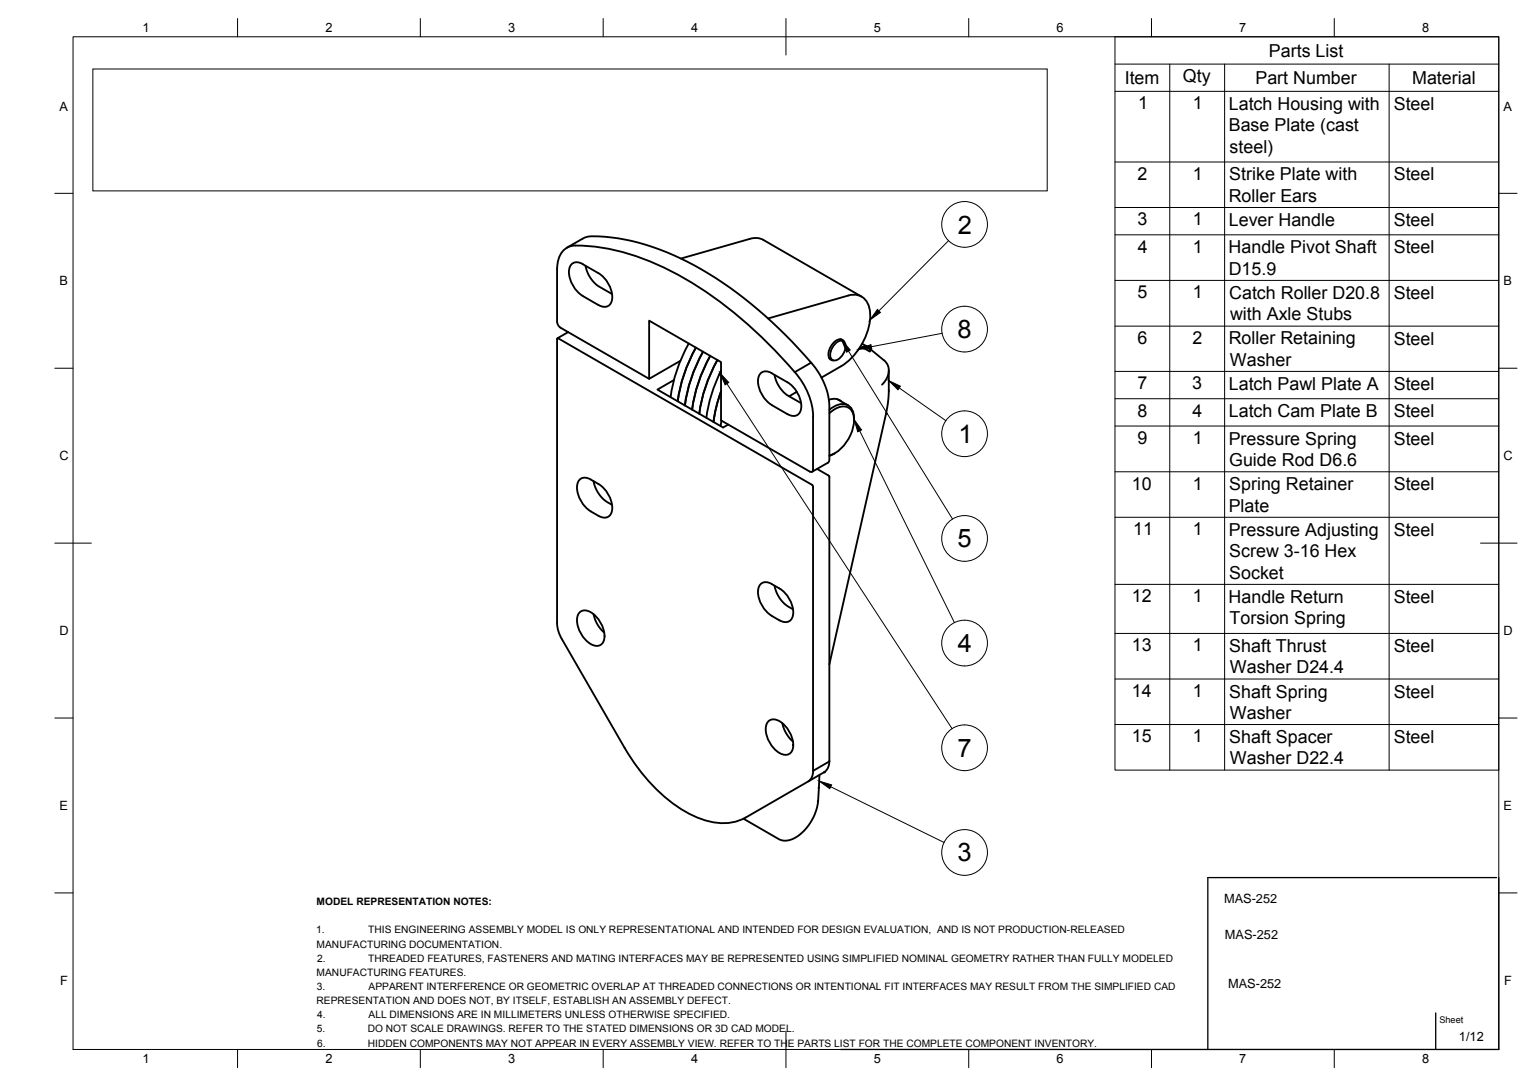
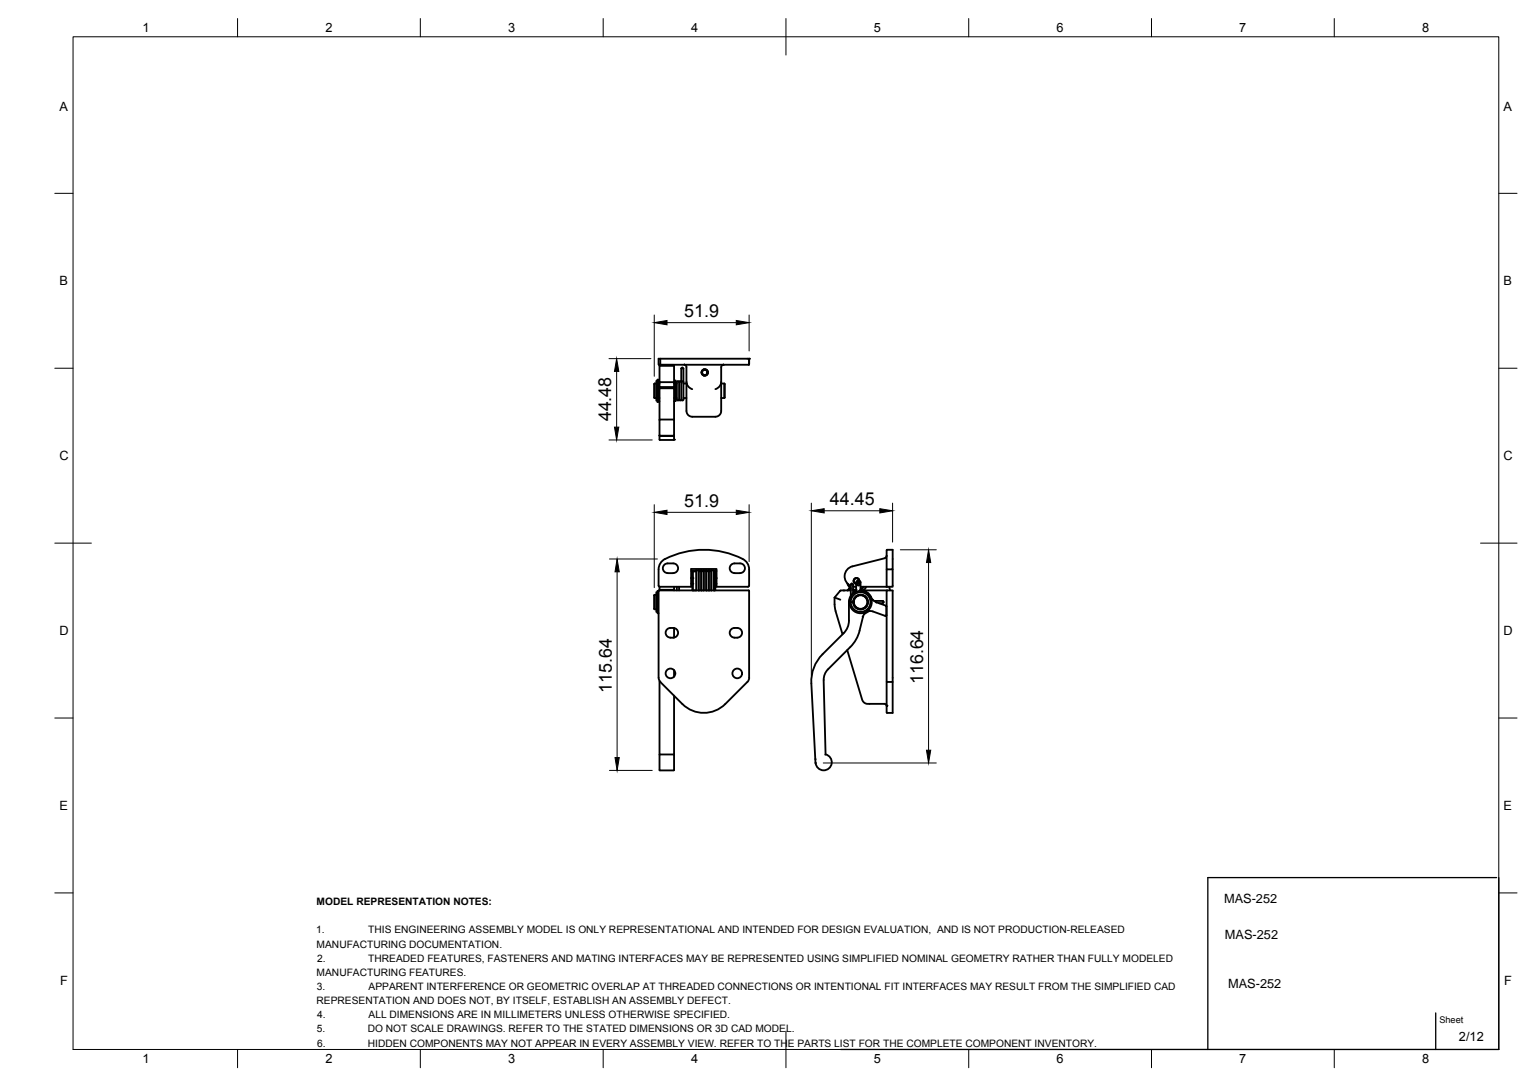
ISO-10303-21;
HEADER;
FILE_DESCRIPTION((''),'2;1');
FILE_NAME('MAS-252','2026-10-06T07:01:46+05:00',(''),(''),'','','');
FILE_SCHEMA (('AUTOMOTIVE_DESIGN { 1 0 10303 214 3 1 1 }'));
ENDSEC;
DATA;
#10 = MECHANICAL_DESIGN_GEOMETRIC_PRESENTATION_REPRESENTATION('',(#138,#139,
#140,#141,#142,#143,#144,#145,#146,#147,#148,#149,#150,#151,#152),#11396) ;
#11 = ITEM_DEFINED_TRANSFORMATION($,$,#5751,#6394) ;
#12 = ITEM_DEFINED_TRANSFORMATION($,$,#5923,#6395) ;
#13 = ITEM_DEFINED_TRANSFORMATION($,$,#6038,#6396) ;
#14 = ITEM_DEFINED_TRANSFORMATION($,$,#6215,#6397) ;
#15 = ITEM_DEFINED_TRANSFORMATION($,$,#6225,#6398) ;
#16 = ITEM_DEFINED_TRANSFORMATION($,$,#6385,#6399) ;
#17 = ITEM_DEFINED_TRANSFORMATION($,$,#6338,#6400) ;
#18 = ITEM_DEFINED_TRANSFORMATION($,$,#6357,#6401) ;
#19 = ITEM_DEFINED_TRANSFORMATION($,$,#6243,#6402) ;
#20 = ITEM_DEFINED_TRANSFORMATION($,$,#6253,#6403) ;
#21 = ITEM_DEFINED_TRANSFORMATION($,$,#6268,#6404) ;
#22 = ITEM_DEFINED_TRANSFORMATION($,$,#6289,#6405) ;
#23 = ITEM_DEFINED_TRANSFORMATION($,$,#6311,#6406) ;
#24 = ITEM_DEFINED_TRANSFORMATION($,$,#6320,#6407) ;
#25 = ITEM_DEFINED_TRANSFORMATION($,$,#6329,#6408) ;
#26 = ITEM_DEFINED_TRANSFORMATION($,$,#6338,#6409) ;
#27 = ITEM_DEFINED_TRANSFORMATION($,$,#6338,#6410) ;
#28 = ITEM_DEFINED_TRANSFORMATION($,$,#6357,#6411) ;
#29 = ITEM_DEFINED_TRANSFORMATION($,$,#6357,#6412) ;
#30 = ITEM_DEFINED_TRANSFORMATION($,$,#6357,#6413) ;
#31 = ITEM_DEFINED_TRANSFORMATION($,$,#6385,#6414) ;
#32 = (
REPRESENTATION_RELATIONSHIP($,$,#11455,#11454)
REPRESENTATION_RELATIONSHIP_WITH_TRANSFORMATION(#11)
SHAPE_REPRESENTATION_RELATIONSHIP()
) ;
#33 = (
REPRESENTATION_RELATIONSHIP($,$,#11456,#11454)
REPRESENTATION_RELATIONSHIP_WITH_TRANSFORMATION(#12)
SHAPE_REPRESENTATION_RELATIONSHIP()
) ;
#34 = (
REPRESENTATION_RELATIONSHIP($,$,#11457,#11454)
REPRESENTATION_RELATIONSHIP_WITH_TRANSFORMATION(#13)
SHAPE_REPRESENTATION_RELATIONSHIP()
) ;
#35 = (
REPRESENTATION_RELATIONSHIP($,$,#11458,#11454)
REPRESENTATION_RELATIONSHIP_WITH_TRANSFORMATION(#14)
SHAPE_REPRESENTATION_RELATIONSHIP()
) ;
#36 = (
REPRESENTATION_RELATIONSHIP($,$,#11459,#11454)
REPRESENTATION_RELATIONSHIP_WITH_TRANSFORMATION(#15)
SHAPE_REPRESENTATION_RELATIONSHIP()
) ;
#37 = (
REPRESENTATION_RELATIONSHIP($,$,#11469,#11454)
REPRESENTATION_RELATIONSHIP_WITH_TRANSFORMATION(#16)
SHAPE_REPRESENTATION_RELATIONSHIP()
) ;
#38 = (
REPRESENTATION_RELATIONSHIP($,$,#11467,#11454)
REPRESENTATION_RELATIONSHIP_WITH_TRANSFORMATION(#17)
SHAPE_REPRESENTATION_RELATIONSHIP()
) ;
#39 = (
REPRESENTATION_RELATIONSHIP($,$,#11468,#11454)
REPRESENTATION_RELATIONSHIP_WITH_TRANSFORMATION(#18)
SHAPE_REPRESENTATION_RELATIONSHIP()
) ;
#40 = (
REPRESENTATION_RELATIONSHIP($,$,#11460,#11454)
REPRESENTATION_RELATIONSHIP_WITH_TRANSFORMATION(#19)
SHAPE_REPRESENTATION_RELATIONSHIP()
) ;
#41 = (
REPRESENTATION_RELATIONSHIP($,$,#11461,#11454)
REPRESENTATION_RELATIONSHIP_WITH_TRANSFORMATION(#20)
SHAPE_REPRESENTATION_RELATIONSHIP()
) ;
#42 = (
REPRESENTATION_RELATIONSHIP($,$,#11462,#11454)
REPRESENTATION_RELATIONSHIP_WITH_TRANSFORMATION(#21)
SHAPE_REPRESENTATION_RELATIONSHIP()
) ;
#43 = (
REPRESENTATION_RELATIONSHIP($,$,#11463,#11454)
REPRESENTATION_RELATIONSHIP_WITH_TRANSFORMATION(#22)
SHAPE_REPRESENTATION_RELATIONSHIP()
) ;
#44 = (
REPRESENTATION_RELATIONSHIP($,$,#11464,#11454)
REPRESENTATION_RELATIONSHIP_WITH_TRANSFORMATION(#23)
SHAPE_REPRESENTATION_RELATIONSHIP()
) ;
#45 = (
REPRESENTATION_RELATIONSHIP($,$,#11465,#11454)
REPRESENTATION_RELATIONSHIP_WITH_TRANSFORMATION(#24)
SHAPE_REPRESENTATION_RELATIONSHIP()
) ;
#46 = (
REPRESENTATION_RELATIONSHIP($,$,#11466,#11454)
REPRESENTATION_RELATIONSHIP_WITH_TRANSFORMATION(#25)
SHAPE_REPRESENTATION_RELATIONSHIP()
) ;
#47 = (
REPRESENTATION_RELATIONSHIP($,$,#11467,#11454)
REPRESENTATION_RELATIONSHIP_WITH_TRANSFORMATION(#26)
SHAPE_REPRESENTATION_RELATIONSHIP()
) ;
#48 = (
REPRESENTATION_RELATIONSHIP($,$,#11467,#11454)
REPRESENTATION_RELATIONSHIP_WITH_TRANSFORMATION(#27)
SHAPE_REPRESENTATION_RELATIONSHIP()
) ;
#49 = (
REPRESENTATION_RELATIONSHIP($,$,#11468,#11454)
REPRESENTATION_RELATIONSHIP_WITH_TRANSFORMATION(#28)
SHAPE_REPRESENTATION_RELATIONSHIP()
) ;
#50 = (
REPRESENTATION_RELATIONSHIP($,$,#11468,#11454)
REPRESENTATION_RELATIONSHIP_WITH_TRANSFORMATION(#29)
SHAPE_REPRESENTATION_RELATIONSHIP()
) ;
#51 = (
REPRESENTATION_RELATIONSHIP($,$,#11468,#11454)
REPRESENTATION_RELATIONSHIP_WITH_TRANSFORMATION(#30)
SHAPE_REPRESENTATION_RELATIONSHIP()
) ;
#52 = (
REPRESENTATION_RELATIONSHIP($,$,#11469,#11454)
REPRESENTATION_RELATIONSHIP_WITH_TRANSFORMATION(#31)
SHAPE_REPRESENTATION_RELATIONSHIP()
) ;
#53 = CONTEXT_DEPENDENT_SHAPE_REPRESENTATION(#32,#11433) ;
#54 = CONTEXT_DEPENDENT_SHAPE_REPRESENTATION(#33,#11434) ;
#55 = CONTEXT_DEPENDENT_SHAPE_REPRESENTATION(#34,#11435) ;
#56 = CONTEXT_DEPENDENT_SHAPE_REPRESENTATION(#35,#11436) ;
#57 = CONTEXT_DEPENDENT_SHAPE_REPRESENTATION(#36,#11437) ;
#58 = CONTEXT_DEPENDENT_SHAPE_REPRESENTATION(#37,#11438) ;
#59 = CONTEXT_DEPENDENT_SHAPE_REPRESENTATION(#38,#11439) ;
#60 = CONTEXT_DEPENDENT_SHAPE_REPRESENTATION(#39,#11440) ;
#61 = CONTEXT_DEPENDENT_SHAPE_REPRESENTATION(#40,#11441) ;
#62 = CONTEXT_DEPENDENT_SHAPE_REPRESENTATION(#41,#11442) ;
#63 = CONTEXT_DEPENDENT_SHAPE_REPRESENTATION(#42,#11443) ;
#64 = CONTEXT_DEPENDENT_SHAPE_REPRESENTATION(#43,#11444) ;
#65 = CONTEXT_DEPENDENT_SHAPE_REPRESENTATION(#44,#11445) ;
#66 = CONTEXT_DEPENDENT_SHAPE_REPRESENTATION(#45,#11446) ;
#67 = CONTEXT_DEPENDENT_SHAPE_REPRESENTATION(#46,#11447) ;
#68 = CONTEXT_DEPENDENT_SHAPE_REPRESENTATION(#47,#11448) ;
#69 = CONTEXT_DEPENDENT_SHAPE_REPRESENTATION(#48,#11449) ;
#70 = CONTEXT_DEPENDENT_SHAPE_REPRESENTATION(#49,#11450) ;
#71 = CONTEXT_DEPENDENT_SHAPE_REPRESENTATION(#50,#11451) ;
#72 = CONTEXT_DEPENDENT_SHAPE_REPRESENTATION(#51,#11452) ;
#73 = CONTEXT_DEPENDENT_SHAPE_REPRESENTATION(#52,#11453) ;
#74 = NEXT_ASSEMBLY_USAGE_OCCURRENCE(
'Latch Housing with Base Plate (cast steel):1',
'Latch Housing with Base Plate (cast steel):1',
'Latch Housing with Base Plate (cast steel):1',#11471,#11472,
'Latch Housing with Base Plate (cast steel):1') ;
#75 = NEXT_ASSEMBLY_USAGE_OCCURRENCE('Strike Plate with Roller Ears:1',
'Strike Plate with Roller Ears:1','Strike Plate with Roller Ears:1',#11471,
#11473,'Strike Plate with Roller Ears:1') ;
#76 = NEXT_ASSEMBLY_USAGE_OCCURRENCE('Lever Handle:1','Lever Handle:1',
'Lever Handle:1',#11471,#11474,'Lever Handle:1') ;
#77 = NEXT_ASSEMBLY_USAGE_OCCURRENCE('Handle Pivot Shaft D15.9:1',
'Handle Pivot Shaft D15.9:1','Handle Pivot Shaft D15.9:1',#11471,#11475,
'Handle Pivot Shaft D15.9:1') ;
#78 = NEXT_ASSEMBLY_USAGE_OCCURRENCE(
'Catch Roller D20.8 with Axle Stubs:1',
'Catch Roller D20.8 with Axle Stubs:1',
'Catch Roller D20.8 with Axle Stubs:1',#11471,#11476,
'Catch Roller D20.8 with Axle Stubs:1') ;
#79 = NEXT_ASSEMBLY_USAGE_OCCURRENCE('Roller Retaining Washer:1',
'Roller Retaining Washer:1','Roller Retaining Washer:1',#11471,#11486,
'Roller Retaining Washer:1') ;
#80 = NEXT_ASSEMBLY_USAGE_OCCURRENCE('Latch Pawl Plate A:1',
'Latch Pawl Plate A:1','Latch Pawl Plate A:1',#11471,#11484,
'Latch Pawl Plate A:1') ;
#81 = NEXT_ASSEMBLY_USAGE_OCCURRENCE('Latch Cam Plate B:1',
'Latch Cam Plate B:1','Latch Cam Plate B:1',#11471,#11485,
'Latch Cam Plate B:1') ;
#82 = NEXT_ASSEMBLY_USAGE_OCCURRENCE('Pressure Spring Guide Rod D6.6:1',
'Pressure Spring Guide Rod D6.6:1','Pressure Spring Guide Rod D6.6:1',#11471,
#11477,'Pressure Spring Guide Rod D6.6:1') ;
#83 = NEXT_ASSEMBLY_USAGE_OCCURRENCE('Spring Retainer Plate:1',
'Spring Retainer Plate:1','Spring Retainer Plate:1',#11471,#11478,
'Spring Retainer Plate:1') ;
#84 = NEXT_ASSEMBLY_USAGE_OCCURRENCE(
'Pressure Adjusting Screw 3-16 Hex Socket:1',
'Pressure Adjusting Screw 3-16 Hex Socket:1',
'Pressure Adjusting Screw 3-16 Hex Socket:1',#11471,#11479,
'Pressure Adjusting Screw 3-16 Hex Socket:1') ;
#85 = NEXT_ASSEMBLY_USAGE_OCCURRENCE('Handle Return Torsion Spring:1',
'Handle Return Torsion Spring:1','Handle Return Torsion Spring:1',#11471,
#11480,'Handle Return Torsion Spring:1') ;
#86 = NEXT_ASSEMBLY_USAGE_OCCURRENCE('Shaft Thrust Washer D24.4:1',
'Shaft Thrust Washer D24.4:1','Shaft Thrust Washer D24.4:1',#11471,#11481,
'Shaft Thrust Washer D24.4:1') ;
#87 = NEXT_ASSEMBLY_USAGE_OCCURRENCE('Shaft Spring Washer:1',
'Shaft Spring Washer:1','Shaft Spring Washer:1',#11471,#11482,
'Shaft Spring Washer:1') ;
#88 = NEXT_ASSEMBLY_USAGE_OCCURRENCE('Shaft Spacer Washer D22.4:1',
'Shaft Spacer Washer D22.4:1','Shaft Spacer Washer D22.4:1',#11471,#11483,
'Shaft Spacer Washer D22.4:1') ;
#89 = NEXT_ASSEMBLY_USAGE_OCCURRENCE('Latch Pawl Plate A:2',
'Latch Pawl Plate A:2','Latch Pawl Plate A:2',#11471,#11484,
'Latch Pawl Plate A:2') ;
#90 = NEXT_ASSEMBLY_USAGE_OCCURRENCE('Latch Pawl Plate A:3',
'Latch Pawl Plate A:3','Latch Pawl Plate A:3',#11471,#11484,
'Latch Pawl Plate A:3') ;
#91 = NEXT_ASSEMBLY_USAGE_OCCURRENCE('Latch Cam Plate B:2',
'Latch Cam Plate B:2','Latch Cam Plate B:2',#11471,#11485,
'Latch Cam Plate B:2') ;
#92 = NEXT_ASSEMBLY_USAGE_OCCURRENCE('Latch Cam Plate B:3',
'Latch Cam Plate B:3','Latch Cam Plate B:3',#11471,#11485,
'Latch Cam Plate B:3') ;
#93 = NEXT_ASSEMBLY_USAGE_OCCURRENCE('Latch Cam Plate B:4',
'Latch Cam Plate B:4','Latch Cam Plate B:4',#11471,#11485,
'Latch Cam Plate B:4') ;
#94 = NEXT_ASSEMBLY_USAGE_OCCURRENCE('Roller Retaining Washer:2',
'Roller Retaining Washer:2','Roller Retaining Washer:2',#11471,#11486,
'Roller Retaining Washer:2') ;
#95 = CONICAL_SURFACE('',#6218,3.825,0.785398163397448) ;
#96 = CONICAL_SURFACE('',#6222,3.825,0.785398163397448) ;
#97 = CONICAL_SURFACE('',#6232,5.05,0.785398163397455) ;
#98 = CONICAL_SURFACE('',#6236,5.05,0.785398163397455) ;
#99 = CONICAL_SURFACE('',#6246,1.525,0.78539816339745) ;
#100 = CONICAL_SURFACE('',#6250,1.525,0.78539816339745) ;
#101 = CONICAL_SURFACE('',#6278,1.80518500301908,0.785398163397443) ;
#102 = CONICAL_SURFACE('',#6282,1.76268064699232,0.75976275487579) ;
#103 = CONICAL_SURFACE('',#6286,1.56015989180596,0.67474094222354) ;
#104 = CONICAL_SURFACE('',#6292,0.605,0.785398163397447) ;
#105 = CONICAL_SURFACE('',#6305,0.605,0.78539816339745) ;
#106 = (
BOUNDED_SURFACE()
B_SPLINE_SURFACE(2,2,((#9482,#9483,#9484),(#9485,#9486,#9487),(#9488,#9489,
#9490)),.UNSPECIFIED.,.F.,.F.,.F.)
B_SPLINE_SURFACE_WITH_KNOTS((3,3),(3,3),(0.,1.5707963267949),(-2.95294089690097,
-1.43909013515432),.UNSPECIFIED.)
GEOMETRIC_REPRESENTATION_ITEM()
RATIONAL_B_SPLINE_SURFACE(((1.,0.726950752418356,1.),(0.707106781186548,
0.514031806623683,0.707106781186548),(1.,0.726950752418356,1.)))
REPRESENTATION_ITEM('')
SURFACE()
) ;
#107 = (
BOUNDED_SURFACE()
B_SPLINE_SURFACE(2,2,((#10602,#10603,#10604),(#10605,#10606,#10607),(#10608,
#10609,#10610)),.UNSPECIFIED.,.F.,.F.,.F.)
B_SPLINE_SURFACE_WITH_KNOTS((3,3),(3,3),(-1.5707963267949,0.),(-2.95294089690006,
-1.43909013515442),.UNSPECIFIED.)
GEOMETRIC_REPRESENTATION_ITEM()
RATIONAL_B_SPLINE_SURFACE(((1.,0.726950752418703,1.),(0.707106781186561,
0.514031806623938,0.707106781186561),(1.,0.726950752418703,1.)))
REPRESENTATION_ITEM('')
SURFACE()
) ;
#108 = SHAPE_REPRESENTATION_RELATIONSHIP('SRR','None',#11455,#123) ;
#109 = SHAPE_REPRESENTATION_RELATIONSHIP('SRR','None',#11456,#124) ;
#110 = SHAPE_REPRESENTATION_RELATIONSHIP('SRR','None',#11457,#125) ;
#111 = SHAPE_REPRESENTATION_RELATIONSHIP('SRR','None',#11458,#126) ;
#112 = SHAPE_REPRESENTATION_RELATIONSHIP('SRR','None',#11459,#127) ;
#113 = SHAPE_REPRESENTATION_RELATIONSHIP('SRR','None',#11460,#128) ;
#114 = SHAPE_REPRESENTATION_RELATIONSHIP('SRR','None',#11461,#129) ;
#115 = SHAPE_REPRESENTATION_RELATIONSHIP('SRR','None',#11462,#130) ;
#116 = SHAPE_REPRESENTATION_RELATIONSHIP('SRR','None',#11463,#131) ;
#117 = SHAPE_REPRESENTATION_RELATIONSHIP('SRR','None',#11464,#132) ;
#118 = SHAPE_REPRESENTATION_RELATIONSHIP('SRR','None',#11465,#133) ;
#119 = SHAPE_REPRESENTATION_RELATIONSHIP('SRR','None',#11466,#134) ;
#120 = SHAPE_REPRESENTATION_RELATIONSHIP('SRR','None',#11467,#135) ;
#121 = SHAPE_REPRESENTATION_RELATIONSHIP('SRR','None',#11468,#136) ;
#122 = SHAPE_REPRESENTATION_RELATIONSHIP('SRR','None',#11469,#137) ;
#123 = ADVANCED_BREP_SHAPE_REPRESENTATION('',(#153),#11381) ;
#124 = ADVANCED_BREP_SHAPE_REPRESENTATION('',(#154),#11382) ;
#125 = ADVANCED_BREP_SHAPE_REPRESENTATION('',(#155),#11383) ;
#126 = ADVANCED_BREP_SHAPE_REPRESENTATION('',(#156),#11384) ;
#127 = ADVANCED_BREP_SHAPE_REPRESENTATION('',(#157),#11385) ;
#128 = ADVANCED_BREP_SHAPE_REPRESENTATION('',(#158),#11386) ;
#129 = ADVANCED_BREP_SHAPE_REPRESENTATION('',(#159),#11387) ;
#130 = ADVANCED_BREP_SHAPE_REPRESENTATION('',(#160),#11388) ;
#131 = ADVANCED_BREP_SHAPE_REPRESENTATION('',(#161),#11389) ;
#132 = ADVANCED_BREP_SHAPE_REPRESENTATION('',(#162),#11390) ;
#133 = ADVANCED_BREP_SHAPE_REPRESENTATION('',(#163),#11391) ;
#134 = ADVANCED_BREP_SHAPE_REPRESENTATION('',(#164),#11392) ;
#135 = ADVANCED_BREP_SHAPE_REPRESENTATION('',(#165),#11393) ;
#136 = ADVANCED_BREP_SHAPE_REPRESENTATION('',(#166),#11394) ;
#137 = ADVANCED_BREP_SHAPE_REPRESENTATION('',(#167),#11395) ;
#138 = STYLED_ITEM('',(#11539),#153) ;
#139 = STYLED_ITEM('',(#11540),#154) ;
#140 = STYLED_ITEM('',(#11541),#155) ;
#141 = STYLED_ITEM('',(#11542),#156) ;
#142 = STYLED_ITEM('',(#11543),#157) ;
#143 = STYLED_ITEM('',(#11544),#158) ;
#144 = STYLED_ITEM('',(#11545),#159) ;
#145 = STYLED_ITEM('',(#11546),#160) ;
#146 = STYLED_ITEM('',(#11547),#161) ;
#147 = STYLED_ITEM('',(#11548),#162) ;
#148 = STYLED_ITEM('',(#11549),#163) ;
#149 = STYLED_ITEM('',(#11550),#164) ;
#150 = STYLED_ITEM('',(#11551),#165) ;
#151 = STYLED_ITEM('',(#11552),#166) ;
#152 = STYLED_ITEM('',(#11553),#167) ;
#153 = MANIFOLD_SOLID_BREP('Latch Housing with Base Plate (cast steel)',#5569) ;
#154 = MANIFOLD_SOLID_BREP('Strike Plate with Roller Ears',#5570) ;
#155 = MANIFOLD_SOLID_BREP('Lever Handle',#5571) ;
#156 = MANIFOLD_SOLID_BREP('Handle Pivot Shaft D15.9',#5572) ;
#157 = MANIFOLD_SOLID_BREP('Catch Roller D20.8 with Axle Stubs',#5573) ;
#158 = MANIFOLD_SOLID_BREP('Pressure Spring Guide Rod D6.6',#5574) ;
#159 = MANIFOLD_SOLID_BREP('Spring Retainer Plate',#5575) ;
#160 = MANIFOLD_SOLID_BREP('Pressure Adjusting Screw 3-16 Hex Socket',#5576) ;
#161 = MANIFOLD_SOLID_BREP('Handle Return Torsion Spring',#5577) ;
#162 = MANIFOLD_SOLID_BREP('Shaft Thrust Washer D24.4',#5578) ;
#163 = MANIFOLD_SOLID_BREP('Shaft Spring Washer',#5579) ;
#164 = MANIFOLD_SOLID_BREP('Shaft Spacer Washer D22.4',#5580) ;
#165 = MANIFOLD_SOLID_BREP('Latch Pawl Plate A',#5581) ;
#166 = MANIFOLD_SOLID_BREP('Latch Cam Plate B',#5582) ;
#167 = MANIFOLD_SOLID_BREP('Roller Retaining Washer',#5583) ;
#168 = SPHERICAL_SURFACE('',#5868,0.25) ;
#169 = SPHERICAL_SURFACE('',#5870,0.25) ;
#170 = B_SPLINE_SURFACE_WITH_KNOTS('',3,3,((#8352,#8353,#8354,#8355,#8356),
(#8357,#8358,#8359,#8360,#8361),(#8362,#8363,#8364,#8365,#8366),(#8367,
#8368,#8369,#8370,#8371),(#8372,#8373,#8374,#8375,#8376)),.UNSPECIFIED.,
 .F.,.F.,.F.,(4,1,4),(4,1,4),(0.,0.5,1.),(0.152021076009298,0.962749790743926,
1.5707963267949),.UNSPECIFIED.) ;
#171 = B_SPLINE_SURFACE_WITH_KNOTS('',3,3,((#8498,#8499,#8500,#8501),(#8502,
#8503,#8504,#8505),(#8506,#8507,#8508,#8509),(#8510,#8511,#8512,#8513),
(#8514,#8515,#8516,#8517)),.UNSPECIFIED.,.F.,.F.,.F.,(4,1,4),(4,4),(0.,
0.5,1.),(0.247286151692027,0.297678176745857),.UNSPECIFIED.) ;
#172 = B_SPLINE_SURFACE_WITH_KNOTS('',3,3,((#8566,#8567,#8568,#8569),(#8570,
#8571,#8572,#8573),(#8574,#8575,#8576,#8577),(#8578,#8579,#8580,#8581),
(#8582,#8583,#8584,#8585)),.UNSPECIFIED.,.F.,.F.,.F.,(4,1,4),(4,4),(0.,
0.5,1.),(0.268639752323811,0.328790837661693),.UNSPECIFIED.) ;
#173 = B_SPLINE_SURFACE_WITH_KNOTS('',3,3,((#8636,#8637,#8638,#8639),(#8640,
#8641,#8642,#8643),(#8644,#8645,#8646,#8647),(#8648,#8649,#8650,#8651),
(#8652,#8653,#8654,#8655)),.UNSPECIFIED.,.F.,.F.,.F.,(4,1,4),(4,4),(0.,
0.5,1.),(8.83098018298437E-16,0.0601510853378708),.UNSPECIFIED.) ;
#174 = B_SPLINE_SURFACE_WITH_KNOTS('',3,3,((#8668,#8669,#8670,#8671),(#8672,
#8673,#8674,#8675),(#8676,#8677,#8678,#8679),(#8680,#8681,#8682,#8683),
(#8684,#8685,#8686,#8687)),.UNSPECIFIED.,.F.,.F.,.F.,(4,1,4),(4,4),(0.,
0.5,1.),(1.40103212881273E-16,0.0503920250538296),.UNSPECIFIED.) ;
#175 = B_SPLINE_SURFACE_WITH_KNOTS('',3,3,((#8744,#8745,#8746,#8747,#8748),
(#8749,#8750,#8751,#8752,#8753),(#8754,#8755,#8756,#8757,#8758),(#8759,
#8760,#8761,#8762,#8763),(#8764,#8765,#8766,#8767,#8768)),.UNSPECIFIED.,
 .F.,.F.,.F.,(4,1,4),(4,1,4),(0.,0.5,1.),(-1.5707963267949,-0.962749790743935,
-0.152021076009317),.UNSPECIFIED.) ;
#176 = TOROIDAL_SURFACE('',#5776,2.915,0.25) ;
#177 = TOROIDAL_SURFACE('',#5783,2.915,0.25) ;
#178 = TOROIDAL_SURFACE('',#5795,2.915,0.25) ;
#179 = TOROIDAL_SURFACE('',#5801,2.915,0.25) ;
#180 = TOROIDAL_SURFACE('',#5813,2.915,0.25) ;
#181 = TOROIDAL_SURFACE('',#5819,2.915,0.25) ;
#182 = TOROIDAL_SURFACE('',#5833,1.52,0.25) ;
#183 = TOROIDAL_SURFACE('',#5836,3.05499364382027,0.25) ;
#184 = TOROIDAL_SURFACE('',#5838,2.83595375255767,0.25) ;
#185 = TOROIDAL_SURFACE('',#5843,16.3358074534161,0.25) ;
#186 = TOROIDAL_SURFACE('',#5847,16.3358074534161,0.25) ;
#187 = TOROIDAL_SURFACE('',#5850,16.3358074534161,0.25) ;
#188 = TOROIDAL_SURFACE('',#5860,1.52,0.25) ;
#189 = TOROIDAL_SURFACE('',#5885,10.1848235398934,3.175) ;
#190 = TOROIDAL_SURFACE('',#5899,10.1848235398934,3.175) ;
#191 = TOROIDAL_SURFACE('',#5927,0.5,0.25) ;
#192 = TOROIDAL_SURFACE('',#5934,0.5,0.25) ;
#193 = TOROIDAL_SURFACE('',#5944,2.915,0.25) ;
#194 = TOROIDAL_SURFACE('',#5951,2.915,0.25) ;
#195 = TOROIDAL_SURFACE('',#5967,2.915,0.25) ;
#196 = TOROIDAL_SURFACE('',#5973,2.915,0.25) ;
#197 = TOROIDAL_SURFACE('',#5982,5.95626157119474,0.25) ;
#198 = TOROIDAL_SURFACE('',#5986,0.399999999999999,0.25) ;
#199 = TOROIDAL_SURFACE('',#5990,6.2066222212067,0.25) ;
#200 = TOROIDAL_SURFACE('',#5993,46.8573015873016,0.25) ;
#201 = TOROIDAL_SURFACE('',#5997,0.400000000000004,0.25) ;
#202 = TOROIDAL_SURFACE('',#6043,5.6095419988581,0.2) ;
#203 = TOROIDAL_SURFACE('',#6047,18.7717409779691,0.2) ;
#204 = TOROIDAL_SURFACE('',#6051,6.02789861439302,0.2) ;
#205 = TOROIDAL_SURFACE('',#6055,0.524935224963979,0.2) ;
#206 = TOROIDAL_SURFACE('',#6061,1.8962519345458,0.2) ;
#207 = TOROIDAL_SURFACE('',#6064,20.567808830506,0.2) ;
#208 = TOROIDAL_SURFACE('',#6067,6.24675996480776,0.2) ;
#209 = TOROIDAL_SURFACE('',#6070,9.77267576253889,0.2) ;
#210 = TOROIDAL_SURFACE('',#6077,1.00004201680672,0.2) ;
#211 = TOROIDAL_SURFACE('',#6080,4.23606098801213,0.2) ;
#212 = TOROIDAL_SURFACE('',#6084,8.13937148944777,0.2) ;
#213 = TOROIDAL_SURFACE('',#6089,3.96067266925812,0.2) ;
#214 = TOROIDAL_SURFACE('',#6093,4.37909654020415,0.2) ;
#215 = TOROIDAL_SURFACE('',#6097,0.274381812079108,0.2) ;
#216 = TOROIDAL_SURFACE('',#6128,0.274381812079108,0.2) ;
#217 = TOROIDAL_SURFACE('',#6131,4.37909654020415,0.2) ;
#218 = TOROIDAL_SURFACE('',#6135,3.96067266925812,0.2) ;
#219 = TOROIDAL_SURFACE('',#6139,8.13937148944777,0.2) ;
#220 = TOROIDAL_SURFACE('',#6144,1.00004201680672,0.2) ;
#221 = TOROIDAL_SURFACE('',#6146,4.23606098801213,0.2) ;
#222 = TOROIDAL_SURFACE('',#6151,9.77267576253889,0.2) ;
#223 = TOROIDAL_SURFACE('',#6156,20.567808830506,0.2) ;
#224 = TOROIDAL_SURFACE('',#6159,6.24675996480776,0.2) ;
#225 = TOROIDAL_SURFACE('',#6162,1.8962519345458,0.2) ;
#226 = TOROIDAL_SURFACE('',#6166,0.524935224963979,0.2) ;
#227 = TOROIDAL_SURFACE('',#6169,18.7717409779691,0.2) ;
#228 = TOROIDAL_SURFACE('',#6172,6.02789861439302,0.2) ;
#229 = TOROIDAL_SURFACE('',#6175,5.6095419988581,0.2) ;
#230 = TOROIDAL_SURFACE('',#6199,0.85017716535433,0.2) ;
#231 = TOROIDAL_SURFACE('',#6202,0.85017716535433,0.2) ;
#232 = TOROIDAL_SURFACE('',#6207,0.85017716535433,0.2) ;
#233 = TOROIDAL_SURFACE('',#6209,0.85017716535433,0.2) ;
#234 = TOROIDAL_SURFACE('',#6293,4.705,0.605) ;
#235 = TOROIDAL_SURFACE('',#6298,4.705,0.605) ;
#236 = TOROIDAL_SURFACE('',#6306,4.705,0.605) ;
#237 = TOROIDAL_SURFACE('',#6309,4.705,0.605) ;
#238 = B_SPLINE_CURVE_WITH_KNOTS('',3,(#8214,#8215,#8216,#8217,#8218,#8219,
#8220,#8221,#8222,#8223,#8224,#8225,#8226,#8227,#8228,#8229,#8230,#8231,
#8232,#8233),.UNSPECIFIED.,.F.,.F.,(4,2,2,2,2,2,2,2,2,4),(0.,0.0540586324971382,
0.123044542764543,0.150581892580095,0.158718681491189,0.16330566431825,
0.166396075956513,0.169257252570085,0.172939173780484,0.178310039493042),
 .UNSPECIFIED.) ;
#239 = B_SPLINE_CURVE_WITH_KNOTS('',3,(#8399,#8400,#8401,#8402,#8403,#8404,
#8405,#8406,#8407,#8408,#8409,#8410,#8411,#8412,#8413,#8414,#8415,#8416,
#8417,#8418,#8419,#8420,#8421,#8422,#8423,#8424,#8425,#8426),
 .UNSPECIFIED.,.F.,.F.,(4,3,3,3,3,3,3,3,3,4),(0.,0.196349544517553,0.384559246386717,
0.572733492677506,0.76087751170374,0.948996522878222,1.13718101963994,1.32530709535773,
1.51344876765349,1.57079635614042),.UNSPECIFIED.) ;
#240 = B_SPLINE_CURVE_WITH_KNOTS('',3,(#8427,#8428,#8429,#8430,#8431,#8432,
#8433,#8434,#8435,#8436,#8437,#8438),.UNSPECIFIED.,.F.,.F.,(4,2,2,2,2,4),
(-0.000461918039195691,0.,0.00963254585094742,0.0193990205733435,0.0291649301246413,
0.0389305592704718),.UNSPECIFIED.) ;
#241 = B_SPLINE_CURVE_WITH_KNOTS('',3,(#8441,#8442,#8443,#8444,#8445,#8446,
#8447,#8448,#8449,#8450,#8451,#8452,#8453,#8454,#8455,#8456,#8457,#8458,
#8459,#8460,#8461,#8462,#8463,#8464,#8465,#8466,#8467,#8468),
 .UNSPECIFIED.,.F.,.F.,(4,3,3,3,3,3,3,3,3,4),(0.,0.196349545007139,0.384559245883083,
0.57273349111916,0.760877509017182,0.94899651898573,1.13718101444157,1.32530708880429,
1.51344875970823,1.57079636005712),.UNSPECIFIED.) ;
#242 = B_SPLINE_CURVE_WITH_KNOTS('',3,(#8470,#8471,#8472,#8473,#8474,#8475,
#8476,#8477,#8478,#8479,#8480,#8481),.UNSPECIFIED.,.F.,.F.,(4,2,2,2,2,4),
(-0.0393922331407002,-0.0389148464755049,-0.0292979433455524,-0.019531495885866,
-0.00976560909452869,0.),.UNSPECIFIED.) ;
#243 = B_SPLINE_CURVE_WITH_KNOTS('',3,(#8485,#8486,#8487,#8488,#8489,#8490,
#8491,#8492,#8493,#8494,#8495,#8496),.UNSPECIFIED.,.F.,.F.,(4,2,2,2,2,4),
(-0.0393901610897999,-0.0388026611771767,-0.0292983305555518,-0.0195322143643491,
-0.00976610536427336,0.),.UNSPECIFIED.) ;
#244 = B_SPLINE_CURVE_WITH_KNOTS('',3,(#8519,#8520,#8521,#8522),
 .UNSPECIFIED.,.F.,.F.,(4,4),(0.247286151692027,0.297678176745857),
 .UNSPECIFIED.) ;
#245 = B_SPLINE_CURVE_WITH_KNOTS('',3,(#8526,#8527,#8528,#8529),
 .UNSPECIFIED.,.F.,.F.,(4,4),(-0.297678176745857,-0.251823353043443),
 .UNSPECIFIED.) ;
#246 = B_SPLINE_CURVE_WITH_KNOTS('',3,(#8531,#8532,#8533,#8534,#8535,#8536,
#8537,#8538,#8539,#8540,#8541,#8542,#8543,#8544,#8545,#8546,#8547,#8548,
#8549,#8550,#8551,#8552,#8553,#8554,#8555,#8556,#8557,#8558,#8559,#8560,
#8561),.UNSPECIFIED.,.F.,.F.,(4,3,3,3,3,3,3,3,3,3,4),(-0.0348625063534064,
-0.0346987118982289,-0.0299534938780202,-0.0270418791157803,-0.0222988095360682,
-0.0194379956728184,-0.0169333679581277,-0.0122101103613041,-0.00963834412463436,
-0.00481917206231718,0.),.UNSPECIFIED.) ;
#247 = B_SPLINE_CURVE_WITH_KNOTS('',3,(#8562,#8563,#8564,#8565),
 .UNSPECIFIED.,.F.,.F.,(4,4),(0.0910103417204836,0.0923523226751523),
 .UNSPECIFIED.) ;
#248 = B_SPLINE_CURVE_WITH_KNOTS('',3,(#8588,#8589,#8590,#8591),
 .UNSPECIFIED.,.F.,.F.,(4,4),(0.268639752323811,0.328790837661693),
 .UNSPECIFIED.) ;
#249 = B_SPLINE_CURVE_WITH_KNOTS('',3,(#8595,#8596,#8597,#8598),
 .UNSPECIFIED.,.F.,.F.,(4,4),(-0.328790837661693,-0.273035259145455),
 .UNSPECIFIED.) ;
#250 = B_SPLINE_CURVE_WITH_KNOTS('',3,(#8599,#8600,#8601,#8602,#8603,#8604,
#8605,#8606,#8607,#8608,#8609,#8610,#8611,#8612,#8613,#8614,#8615,#8616,
#8617,#8618,#8619,#8620,#8621,#8622,#8623,#8624,#8625,#8626,#8627,#8628,
#8629),.UNSPECIFIED.,.F.,.F.,(4,3,3,3,3,3,3,3,3,3,4),(-0.000163872705022366,
0.,0.00475051443863407,0.00766049069720532,0.0124072603708054,0.0152680067602041,
0.017390180489341,0.0221174050715347,0.0250723399175726,0.0298938142536046,
0.0347152885896365),.UNSPECIFIED.) ;
#251 = B_SPLINE_CURVE_WITH_KNOTS('',3,(#8656,#8657,#8658,#8659),
 .UNSPECIFIED.,.F.,.F.,(4,4),(-0.0557555785162243,-8.83098018298437E-16),
 .UNSPECIFIED.) ;
#252 = B_SPLINE_CURVE_WITH_KNOTS('',3,(#8660,#8661,#8662,#8663),
 .UNSPECIFIED.,.F.,.F.,(4,4),(8.83098018298437E-16,0.0601510853378708),
 .UNSPECIFIED.) ;
#253 = B_SPLINE_CURVE_WITH_KNOTS('',3,(#8688,#8689,#8690,#8691),
 .UNSPECIFIED.,.F.,.F.,(4,4),(-0.0458548237024101,-1.40103212881273E-16),
 .UNSPECIFIED.) ;
#254 = B_SPLINE_CURVE_WITH_KNOTS('',3,(#8693,#8694,#8695,#8696),
 .UNSPECIFIED.,.F.,.F.,(4,4),(1.40103212881273E-16,0.0503920250538296),
 .UNSPECIFIED.) ;
#255 = B_SPLINE_CURVE_WITH_KNOTS('',3,(#8697,#8698,#8699,#8700),
 .UNSPECIFIED.,.F.,.F.,(4,4),(0.,0.00076501868574839),.UNSPECIFIED.) ;
#256 = B_SPLINE_CURVE_WITH_KNOTS('',3,(#8704,#8705,#8706,#8707,#8708,#8709,
#8710,#8711,#8712,#8713,#8714,#8715),.UNSPECIFIED.,.F.,.F.,(4,2,2,2,2,4),
(-0.00058749989859564,0.,0.00950433039685776,0.019270446358007,0.0290365551280728,
0.0388026602624192),.UNSPECIFIED.) ;
#257 = B_SPLINE_CURVE_WITH_KNOTS('',3,(#8771,#8772,#8773,#8774,#8775,#8776,
#8777,#8778,#8779,#8780,#8781,#8782,#8783,#8784,#8785,#8786,#8787,#8788,
#8789,#8790),.UNSPECIFIED.,.F.,.F.,(4,2,2,2,2,2,2,2,2,4),(0.,0.00187316890925574,
0.00298322418909923,0.00385163372182826,0.00475787590428727,0.00612708715977988,
0.00905111735916402,0.0164269109230864,0.0329222866646951,0.0555625738155659),
 .UNSPECIFIED.) ;
#258 = B_SPLINE_CURVE_WITH_KNOTS('',3,(#8834,#8835,#8836,#8837,#8838,#8839,
#8840,#8841,#8842,#8843,#8844,#8845,#8846,#8847,#8848,#8849,#8850,#8851,
#8852,#8853,#8854,#8855,#8856,#8857,#8858,#8859,#8860,#8861,#8862,#8863,
#8864,#8865,#8866,#8867,#8868,#8869,#8870,#8871,#8872,#8873,#8874,#8875,
#8876,#8877,#8878,#8879,#8880,#8881,#8882),.UNSPECIFIED.,.F.,.F.,(4,3,3,
3,3,3,3,3,3,3,3,3,3,3,3,3,4),(0.,0.09964938522947,0.199295818282578,0.298939491768606,
0.39858059832873,0.498219330669901,0.597855881594742,0.697490444026332,
0.797123211027307,0.896771849198539,0.996414865845315,1.09605303531753,
1.19568713170185,1.29533435965265,1.39497149040076,1.4946160591622,1.57079725751296),
 .UNSPECIFIED.) ;
#259 = B_SPLINE_CURVE_WITH_KNOTS('',3,(#8883,#8884,#8885,#8886,#8887,#8888,
#8889,#8890,#8891,#8892,#8893,#8894,#8895,#8896,#8897,#8898,#8899,#8900),
 .UNSPECIFIED.,.F.,.F.,(4,2,2,2,2,2,2,2,4),(-0.00724818355843104,0.,0.00866972814024576,
0.0246774186784591,0.0566526412437171,0.120620928432891,0.244650657098656,
0.368680208659511,0.492709676950837),.UNSPECIFIED.) ;
#260 = B_SPLINE_CURVE_WITH_KNOTS('',3,(#8907,#8908,#8909,#8910,#8911,#8912,
#8913,#8914,#8915,#8916,#8917,#8918,#8919,#8920,#8921,#8922,#8923,#8924,
#8925,#8926,#8927,#8928),.UNSPECIFIED.,.F.,.F.,(4,2,2,2,2,2,2,2,2,2,4),
(0.656794478552693,0.697723395150039,0.83000632281984,1.01882918615295,
1.1132406178195,1.16044633365278,1.18404919156942,1.19585062052774,1.2017513350069,
1.20470169224648,1.20765204948606),.UNSPECIFIED.) ;
#261 = B_SPLINE_CURVE_WITH_KNOTS('',3,(#8947,#8948,#8949,#8950,#8951,#8952,
#8953,#8954,#8955,#8956,#8957,#8958,#8959,#8960,#8961,#8962,#8963,#8964,
#8965,#8966,#8967,#8968),.UNSPECIFIED.,.F.,.F.,(4,2,2,2,2,2,2,2,2,2,4),
(1.20765204948607,1.21060240672565,1.21355276396523,1.21945347844439,1.2312549074027,
1.25485776531934,1.30206348115262,1.39647491281918,1.58529777615229,1.71758070382209,
1.75850962041944),.UNSPECIFIED.) ;
#262 = B_SPLINE_CURVE_WITH_KNOTS('',3,(#8971,#8972,#8973,#8974,#8975,#8976,
#8977,#8978,#8979,#8980,#8981,#8982,#8983,#8984,#8985,#8986,#8987,#8988),
 .UNSPECIFIED.,.F.,.F.,(4,2,2,2,2,2,2,2,4),(-0.499957830797754,-0.492709647672271,
-0.484039920050198,-0.468032230464552,-0.436057009799713,-0.372088726411136,
-0.248059005111197,-0.124029460922085,0.),.UNSPECIFIED.) ;
#263 = B_SPLINE_CURVE_WITH_KNOTS('',3,(#8990,#8991,#8992,#8993,#8994,#8995,
#8996,#8997,#8998,#8999,#9000,#9001,#9002,#9003,#9004,#9005,#9006,#9007,
#9008,#9009,#9010,#9011,#9012,#9013,#9014,#9015,#9016,#9017,#9018,#9019,
#9020,#9021,#9022,#9023,#9024,#9025,#9026,#9027,#9028,#9029,#9030,#9031,
#9032,#9033,#9034,#9035,#9036,#9037,#9038),.UNSPECIFIED.,.F.,.F.,(4,3,3,
3,3,3,3,3,3,3,3,3,3,3,3,3,4),(0.,0.0996501112039543,0.199297271810784,0.298941675382784,
0.398583515425884,0.498222985393558,0.597860278690689,0.697495588677662,
0.797129108674119,0.896778508053707,0.996422290829433,1.09606123100929,
1.19569610220027,1.29534410980026,1.39498202233642,1.4946273745031,1.57080590414797),
 .UNSPECIFIED.) ;
#264 = B_SPLINE_CURVE_WITH_KNOTS('',3,(#9098,#9099,#9100,#9101,#9102,#9103,
#9104,#9105,#9106,#9107),.UNSPECIFIED.,.F.,.F.,(4,2,2,2,4),(0.129530190393873,
0.134403051839659,0.157131608255379,0.18177331440849,0.206415020561601),
 .UNSPECIFIED.) ;
#265 = B_SPLINE_CURVE_WITH_KNOTS('',3,(#9118,#9119,#9120,#9121,#9122,#9123),
 .UNSPECIFIED.,.F.,.F.,(4,2,4),(0.126383060009627,0.145498866650295,0.174889571433522),
 .UNSPECIFIED.) ;
#266 = B_SPLINE_CURVE_WITH_KNOTS('',3,(#9143,#9144,#9145,#9146,#9147,#9148),
 .UNSPECIFIED.,.F.,.F.,(4,2,4),(0.,0.029390704783227,0.0485065114238945),
 .UNSPECIFIED.) ;
#267 = B_SPLINE_CURVE_WITH_KNOTS('',3,(#9157,#9158,#9159,#9160,#9161,#9162,
#9163,#9164,#9165,#9166),.UNSPECIFIED.,.F.,.F.,(4,2,2,2,4),(0.176028199507442,
0.200669905660553,0.225311611813664,0.248040168229384,0.252913029669695),
 .UNSPECIFIED.) ;
#268 = B_SPLINE_CURVE_WITH_KNOTS('',3,(#9272,#9273,#9274,#9275,#9276,#9277,
#9278,#9279,#9280,#9281,#9282,#9283,#9284,#9285,#9286,#9287,#9288,#9289,
#9290,#9291,#9292,#9293,#9294,#9295,#9296,#9297,#9298,#9299),
 .UNSPECIFIED.,.F.,.F.,(4,3,3,3,3,3,3,3,3,4),(0.,0.196349541608207,0.38455924937953,
0.572733501937903,0.760877527668503,0.94899654600919,1.13718105053103,1.32530713430129,
1.51344881486777,1.57079633286566),.UNSPECIFIED.) ;
#269 = B_SPLINE_CURVE_WITH_KNOTS('',3,(#9300,#9301,#9302,#9303,#9304,#9305,
#9306,#9307,#9308,#9309,#9310,#9311),.UNSPECIFIED.,.F.,.F.,(4,2,2,2,2,4),
(-0.0393939259354007,-0.0390590563554235,-0.0292978040547258,-0.0195312295441399,
-0.00976542256445868,0.),.UNSPECIFIED.) ;
#270 = B_SPLINE_CURVE_WITH_KNOTS('',3,(#9327,#9328,#9329,#9330,#9331,#9332,
#9333,#9334,#9335,#9336,#9337,#9338),.UNSPECIFIED.,.F.,.F.,(4,2,2,2,2,4),
(-0.000371179043213308,0.,0.00972368624128075,0.0194900624985635,0.0292560287472632,
0.039021789210692),.UNSPECIFIED.) ;
#271 = B_SPLINE_CURVE_WITH_KNOTS('',3,(#9456,#9457,#9458,#9459,#9460,#9461,
#9462,#9463,#9464,#9465,#9466,#9467),.UNSPECIFIED.,.F.,.F.,(4,2,2,2,2,4),
(-0.000425934342717597,0.,0.00767782768113804,0.0154936481323793,0.0233033297268441,
0.0311102612476663),.UNSPECIFIED.) ;
#272 = B_SPLINE_CURVE_WITH_KNOTS('',3,(#9470,#9471,#9472,#9473,#9474,#9475,
#9476,#9477,#9478,#9479,#9480,#9481),.UNSPECIFIED.,.F.,.F.,(4,2,2,2,2,4),
(-0.000392646763472729,0.,0.00776851635729194,0.0155945832419373,0.0233973193253328,
0.0311896776950334),.UNSPECIFIED.) ;
#273 = B_SPLINE_CURVE_WITH_KNOTS('',3,(#9494,#9495,#9496,#9497,#9498,#9499,
#9500,#9501,#9502,#9503,#9504,#9505),.UNSPECIFIED.,.F.,.F.,(4,2,2,2,2,4),
(-0.0626678583597519,-0.0622419978775531,-0.0545506208202995,-0.046733489174686,
-0.0389252522766465,-0.0311209989394379),.UNSPECIFIED.) ;
#274 = B_SPLINE_CURVE_WITH_KNOTS('',3,(#9511,#9512,#9513,#9514,#9515,#9516,
#9517,#9518,#9519,#9520,#9521,#9522),.UNSPECIFIED.,.F.,.F.,(4,2,2,2,2,4),
(-0.00029630356009181,0.,0.00778002873103429,0.0155932483092341,0.0234059593652307,
0.0312184094334333),.UNSPECIFIED.) ;
#275 = B_SPLINE_CURVE_WITH_KNOTS('',3,(#9528,#9529,#9530,#9531,#9532,#9533,
#9534,#9535,#9536,#9537,#9538,#9539),.UNSPECIFIED.,.F.,.F.,(4,2,2,2,2,4),
(-0.0629385074257631,-0.0627334798904802,-0.0547568943966375,-0.046925593190769,
-0.0391229130222982,-0.0313664342990436),.UNSPECIFIED.) ;
#276 = B_SPLINE_CURVE_WITH_KNOTS('',3,(#9545,#9546,#9547,#9548,#9549,#9550,
#9551,#9552,#9553,#9554,#9555,#9556),.UNSPECIFIED.,.F.,.F.,(4,2,2,2,2,4),
(-0.000203756697037429,0.,0.00796770405795475,0.0158037932485574,0.0236037819491495,
0.031385705039184),.UNSPECIFIED.) ;
#277 = B_SPLINE_CURVE_WITH_KNOTS('',3,(#9561,#9562,#9563,#9564,#9565,#9566,
#9567,#9568,#9569,#9570,#9571,#9572,#9573,#9574,#9575,#9576,#9577,#9578,
#9579,#9580,#9581,#9582,#9583,#9584,#9585),.UNSPECIFIED.,.F.,.F.,(4,3,3,
3,3,3,3,3,4),(0.,0.199052542232163,0.398059502796862,0.597027074925485,
0.795961438809451,0.995008849549264,1.19397259651743,1.39300992499601,1.57079632692443),
 .UNSPECIFIED.) ;
#278 = B_SPLINE_CURVE_WITH_KNOTS('',3,(#9589,#9590,#9591,#9592,#9593,#9594,
#9595,#9596,#9597,#9598,#9599,#9600),.UNSPECIFIED.,.F.,.F.,(4,2,2,2,2,4),
(-0.000302162807502731,0.,0.00777281639954654,0.0155857029470102,0.0233985882068449,
0.0312114728139599),.UNSPECIFIED.) ;
#279 = B_SPLINE_CURVE_WITH_KNOTS('',3,(#9607,#9608,#9609,#9610,#9611,#9612,
#9613,#9614,#9615,#9616,#9617,#9618),.UNSPECIFIED.,.F.,.F.,(4,2,2,2,2,4),
(-0.0315148928540183,-0.0312005996265522,-0.0234381588919511,-0.0156248125751573,
-0.00781221363393156,0.),.UNSPECIFIED.) ;
#280 = B_SPLINE_CURVE_WITH_KNOTS('',3,(#9623,#9624,#9625,#9626,#9627,#9628,
#9629,#9630,#9631,#9632,#9633,#9634),.UNSPECIFIED.,.F.,.F.,(4,2,2,2,2,4),
(-0.000209158996821947,0.,0.00790322324693375,0.0157271724669949,0.0235347393467978,
0.0313323503074072),.UNSPECIFIED.) ;
#281 = B_SPLINE_CURVE_WITH_KNOTS('',3,(#9640,#9641,#9642,#9643,#9644,#9645,
#9646,#9647,#9648,#9649,#9650,#9651,#9652,#9653,#9654,#9655,#9656,#9657,
#9658,#9659,#9660,#9661,#9662,#9663,#9664),.UNSPECIFIED.,.F.,.F.,(4,3,3,
3,3,3,3,3,4),(0.,0.199052706978784,0.398059832253966,0.597027569062776,
0.7959620976022,0.99500967309516,1.19397358474941,1.39301107797699,1.57079762660799),
 .UNSPECIFIED.) ;
#282 = B_SPLINE_CURVE_WITH_KNOTS('',3,(#9670,#9671,#9672,#9673,#9674,#9675,
#9676,#9677,#9678,#9679,#9680,#9681),.UNSPECIFIED.,.F.,.F.,(4,2,2,2,2,4),
(-0.000508786942166875,0.,0.00757813380105505,0.0153951238953111,0.0232058288277231,
0.0310129102887088),.UNSPECIFIED.) ;
#283 = B_SPLINE_CURVE_WITH_KNOTS('',3,(#9686,#9687,#9688,#9689,#9690,#9691,
#9692,#9693,#9694,#9695,#9696,#9697,#9698,#9699,#9700,#9701,#9702,#9703,
#9704,#9705,#9706,#9707,#9708,#9709,#9710),.UNSPECIFIED.,.F.,.F.,(4,3,3,
3,3,3,3,3,4),(0.,0.199053248397837,0.398060914968089,0.597029192964828,
0.79596426260186,0.995012379499913,1.1939768323317,1.39301486693695,1.57080189914441),
 .UNSPECIFIED.) ;
#284 = B_SPLINE_CURVE_WITH_KNOTS('',3,(#9714,#9715,#9716,#9717,#9718,#9719,
#9720,#9721,#9722,#9723,#9724,#9725,#9726,#9727,#9728,#9729),
 .UNSPECIFIED.,.F.,.F.,(4,2,2,2,2,2,2,4),(-0.00032358937009677,0.,0.00354444219611517,
0.00767686671153501,0.0154916858096829,0.0233035611079842,0.0311138771958668,
0.0311774645866534),.UNSPECIFIED.) ;
#285 = B_SPLINE_CURVE_WITH_KNOTS('',3,(#9736,#9737,#9738,#9739,#9740,#9741,
#9742,#9743,#9744,#9745,#9746,#9747,#9748,#9749,#9750,#9751,#9752,#9753,
#9754,#9755,#9756,#9757,#9758,#9759,#9760),.UNSPECIFIED.,.F.,.F.,(4,3,3,
3,3,3,3,3,4),(0.,0.199052583563084,0.398059585450825,0.597027198896615,
0.795961604093608,0.99500905617405,1.19397284446766,1.39301021428897,1.57079665269337),
 .UNSPECIFIED.) ;
#286 = B_SPLINE_CURVE_WITH_KNOTS('',3,(#9768,#9769,#9770,#9771,#9772,#9773,
#9774,#9775,#9776,#9777,#9778,#9779),.UNSPECIFIED.,.F.,.F.,(4,2,2,2,2,4),
(-0.0315123462948468,-0.031000483210486,-0.0234384406752481,-0.0156253470993035,
-0.00781258687358792,0.),.UNSPECIFIED.) ;
#287 = B_SPLINE_CURVE_WITH_KNOTS('',3,(#9785,#9786,#9787,#9788,#9789,#9790,
#9791,#9792,#9793,#9794,#9795,#9796,#9797,#9798,#9799,#9800,#9801,#9802,
#9803,#9804,#9805,#9806,#9807,#9808,#9809),.UNSPECIFIED.,.F.,.F.,(4,3,3,
3,3,3,3,3,4),(0.,0.199052542245368,0.398059502823902,0.59702707496727,0.795961438867092,
0.9950088496244,1.19397259661093,1.39300992510867,1.57079632687287),
 .UNSPECIFIED.) ;
#288 = B_SPLINE_CURVE_WITH_KNOTS('',3,(#9815,#9816,#9817,#9818,#9819,#9820,
#9821,#9822,#9823,#9824,#9825,#9826),.UNSPECIFIED.,.F.,.F.,(4,2,2,2,2,4),
(-0.000472807702419667,0.,0.00760072048225168,0.0154136353110866,0.0232265107396055,
0.0310393663455244),.UNSPECIFIED.) ;
#289 = B_SPLINE_CURVE_WITH_KNOTS('',3,(#9831,#9832,#9833,#9834,#9835,#9836,
#9837,#9838,#9839,#9840,#9841,#9842,#9843,#9844,#9845,#9846,#9847,#9848,
#9849,#9850,#9851,#9852,#9853,#9854,#9855),.UNSPECIFIED.,.F.,.F.,(4,3,3,
3,3,3,3,3,4),(0.,0.199052542243981,0.398059502821061,0.597027074962877,
0.795961438861017,0.995008849616485,1.19397259660109,1.39300992509683,1.57079632687829),
 .UNSPECIFIED.) ;
#290 = B_SPLINE_CURVE_WITH_KNOTS('',3,(#9872,#9873,#9874,#9875,#9876,#9877,
#9878,#9879,#9880,#9881,#9882,#9883),.UNSPECIFIED.,.F.,.F.,(4,2,2,2,2,4),
(-0.0315141126684919,-0.031176944954667,-0.0234383818709659,-0.0156252430234338,
-0.00781251789292829,0.),.UNSPECIFIED.) ;
#291 = B_SPLINE_CURVE_WITH_KNOTS('',3,(#9887,#9888,#9889,#9890,#9891,#9892,
#9893,#9894,#9895,#9896,#9897,#9898,#9899,#9900,#9901,#9902,#9903,#9904,
#9905,#9906,#9907,#9908,#9909,#9910,#9911),.UNSPECIFIED.,.F.,.F.,(4,3,3,
3,3,3,3,3,4),(0.,0.199052485193076,0.398059386004224,0.597026894426605,
0.795961189880508,0.995008525064052,1.19397219273933,1.39300943847609,1.57079654966886),
 .UNSPECIFIED.) ;
#292 = B_SPLINE_CURVE_WITH_KNOTS('',3,(#9919,#9920,#9921,#9922,#9923,#9924,
#9925,#9926,#9927,#9928,#9929,#9930,#9931,#9932),.UNSPECIFIED.,.F.,.F.,
(4,2,2,2,2,2,4),(-0.071485180683264,-0.0712307719726932,-0.064253173333706,
-0.0574900962687512,-0.0489313629526751,-0.0419539746827257,-0.0356153859867279),
 .UNSPECIFIED.) ;
#293 = B_SPLINE_CURVE_WITH_KNOTS('',3,(#9950,#9951,#9952,#9953,#9954,#9955,
#9956,#9957,#9958,#9959,#9960,#9961,#9962,#9963),.UNSPECIFIED.,.F.,.F.,
(4,2,2,2,2,2,4),(-0.063419024433945,-0.0632138433555934,-0.0550363404792558,
-0.0471273977752151,-0.0393668335371398,-0.0316820163148599,-0.0316075730538707),
 .UNSPECIFIED.) ;
#294 = B_SPLINE_CURVE_WITH_KNOTS('',3,(#9969,#9970,#9971,#9972,#9973,#9974,
#9975,#9976,#9977,#9978,#9979,#9980,#9981,#9982),.UNSPECIFIED.,.F.,.F.,
(4,2,2,2,2,2,4),(-0.000204835146312565,0.,0.00817143806143788,0.0160775285373022,
0.0238394400759123,0.0315278536559536,0.0315985683409222),.UNSPECIFIED.) ;
#295 = B_SPLINE_CURVE_WITH_KNOTS('',3,(#9987,#9988,#9989,#9990,#9991,#9992,
#9993,#9994,#9995,#9996,#9997,#9998,#9999,#10000),.UNSPECIFIED.,.F.,.F.,
(4,2,2,2,2,2,4),(-0.0315119651507534,-0.0310369720406695,-0.0234522322979694,
-0.0156393394528541,-0.00782644846731675,-1.35584415946594E-5,0.),
 .UNSPECIFIED.) ;
#296 = B_SPLINE_CURVE_WITH_KNOTS('',3,(#10007,#10008,#10009,#10010,#10011,
#10012,#10013,#10014,#10015,#10016,#10017,#10018),.UNSPECIFIED.,.F.,.F.,
(4,2,2,2,2,4),(-0.031721691652862,-0.0314189347322439,-0.0233633267396854,
-0.0155133765946492,-0.00773979585571865,0.),.UNSPECIFIED.) ;
#297 = B_SPLINE_CURVE_WITH_KNOTS('',3,(#10099,#10100,#10101,#10102,#10103,
#10104,#10105,#10106,#10107,#10108,#10109,#10110),.UNSPECIFIED.,.F.,.F.,
(4,2,2,2,2,4),(-0.000302979244329871,0.,0.00806152347440571,0.0159172380801614,
0.0236965271994009,0.0314420066261495),.UNSPECIFIED.) ;
#298 = B_SPLINE_CURVE_WITH_KNOTS('',3,(#10111,#10112,#10113,#10114,#10115,
#10116,#10117,#10118,#10119,#10120,#10121,#10122),.UNSPECIFIED.,.F.,.F.,
(4,2,2,2,2,4),(-0.0315754136058091,-0.0311828527614278,-0.0234160363129251,
-0.0155916819303375,-0.00779065324374899,0.),.UNSPECIFIED.) ;
#299 = B_SPLINE_CURVE_WITH_KNOTS('',3,(#10127,#10128,#10129,#10130,#10131,
#10132,#10133,#10134,#10135,#10136,#10137,#10138,#10139,#10140),
 .UNSPECIFIED.,.F.,.F.,(4,2,2,2,2,2,4),(-0.000474992982336123,0.,0.00758473725973339,
0.0153976269864644,0.0232105148526209,0.0310234017590763,0.0310369601957522),
 .UNSPECIFIED.) ;
#300 = B_SPLINE_CURVE_WITH_KNOTS('',3,(#10146,#10147,#10148,#10149,#10150,
#10151,#10152,#10153,#10154,#10155,#10156,#10157),.UNSPECIFIED.,.F.,.F.,
(4,2,2,2,2,4),(-0.0634032075025796,-0.0631983745559419,-0.0551219653781809,
-0.0471164301307063,-0.039256298781182,-0.0315985683616453),
 .UNSPECIFIED.) ;
#301 = B_SPLINE_CURVE_WITH_KNOTS('',3,(#10163,#10164,#10165,#10166,#10167,
#10168,#10169,#10170,#10171,#10172,#10173,#10174),.UNSPECIFIED.,.F.,.F.,
(4,2,2,2,2,4),(-0.000205178731636372,0.,0.00808313825878162,0.0160941684934645,
0.0239559117961846,0.0316075730471855),.UNSPECIFIED.) ;
#302 = B_SPLINE_CURVE_WITH_KNOTS('',3,(#10180,#10181,#10182,#10183,#10184,
#10185,#10186,#10187,#10188,#10189,#10190,#10191),.UNSPECIFIED.,.F.,.F.,
(4,2,2,2,2,4),(-0.000314294385248188,0.,0.00776246933425461,0.0155758444397962,
0.0233884721670194,0.0312007145855276),.UNSPECIFIED.) ;
#303 = B_SPLINE_CURVE_WITH_KNOTS('',3,(#10195,#10196,#10197,#10198,#10199,
#10200,#10201,#10202,#10203,#10204,#10205,#10206,#10207,#10208,#10209,#10210,
#10211,#10212,#10213,#10214,#10215,#10216,#10217,#10218,#10219),
 .UNSPECIFIED.,.F.,.F.,(4,3,3,3,3,3,3,3,4),(0.,0.199053248397837,0.398060914968088,
0.597029192964836,0.795964262601867,0.995012379499923,1.19397683233171,
1.39301486693695,1.57080189914441),.UNSPECIFIED.) ;
#304 = B_SPLINE_CURVE_WITH_KNOTS('',3,(#10222,#10223,#10224,#10225,#10226,
#10227,#10228,#10229,#10230,#10231,#10232,#10233),.UNSPECIFIED.,.F.,.F.,
(4,2,2,2,2,4),(-0.0315210097541554,-0.0310122339084761,-0.0234342653837737,
-0.0156174457752067,-0.00780691119140275,0.),.UNSPECIFIED.) ;
#305 = B_SPLINE_CURVE_WITH_KNOTS('',3,(#10237,#10238,#10239,#10240,#10241,
#10242,#10243,#10244,#10245,#10246,#10247,#10248,#10249,#10250,#10251,#10252,
#10253,#10254,#10255,#10256,#10257,#10258,#10259,#10260,#10261),
 .UNSPECIFIED.,.F.,.F.,(4,3,3,3,3,3,3,3,4),(0.,0.199052542064369,0.398059502453293,
0.597027074394497,0.795961438077169,0.995008848594717,1.19397259532962,
1.39300992356481,1.57079632757971),.UNSPECIFIED.) ;
#306 = B_SPLINE_CURVE_WITH_KNOTS('',3,(#10272,#10273,#10274,#10275,#10276,
#10277,#10278,#10279,#10280,#10281,#10282,#10283,#10284,#10285),
 .UNSPECIFIED.,.F.,.F.,(4,2,2,2,2,2,4),(-0.000254408710349561,0.,0.00697759863796767,
0.0137406757011616,0.0222994090150433,0.0292767972832062,0.035615385977577),
 .UNSPECIFIED.) ;
#307 = B_SPLINE_CURVE_WITH_KNOTS('',3,(#10288,#10289,#10290,#10291,#10292,
#10293,#10294,#10295,#10296,#10297,#10298,#10299,#10300,#10301,#10302,#10303,
#10304,#10305,#10306,#10307,#10308,#10309,#10310,#10311,#10312),
 .UNSPECIFIED.,.F.,.F.,(4,3,3,3,3,3,3,3,4),(0.,0.199052485193076,0.398059386004222,
0.597026894426605,0.795961189880508,0.995008525064048,1.19397219273933,
1.39300943847609,1.57079654966886),.UNSPECIFIED.) ;
#308 = B_SPLINE_CURVE_WITH_KNOTS('',3,(#10318,#10319,#10320,#10321,#10322,
#10323,#10324,#10325,#10326,#10327,#10328,#10329),.UNSPECIFIED.,.F.,.F.,
(4,2,2,2,2,4),(-0.000337168458022535,0.,0.00773858016387553,0.0155517362556591,
0.0233644786295,0.031177013765312),.UNSPECIFIED.) ;
#309 = B_SPLINE_CURVE_WITH_KNOTS('',3,(#10339,#10340,#10341,#10342,#10343,
#10344,#10345,#10346,#10347,#10348,#10349,#10350,#10351,#10352,#10353,#10354,
#10355,#10356,#10357,#10358,#10359,#10360,#10361,#10362,#10363),
 .UNSPECIFIED.,.F.,.F.,(4,3,3,3,3,3,3,3,4),(0.,0.199052542234199,0.398059502803477,
0.597027074940396,0.795961438837137,0.995008849596832,1.1939725965883,1.39300992509389,
1.57079632687829),.UNSPECIFIED.) ;
#310 = B_SPLINE_CURVE_WITH_KNOTS('',3,(#10370,#10371,#10372,#10373,#10374,
#10375,#10376,#10377,#10378,#10379,#10380,#10381,#10382,#10383,#10384,#10385,
#10386,#10387,#10388,#10389,#10390,#10391,#10392,#10393,#10394),
 .UNSPECIFIED.,.F.,.F.,(4,3,3,3,3,3,3,3,4),(0.,0.199052646770473,0.398059711851129,
0.597027388477328,0.795961856844187,0.99500937213039,1.19397322360319,1.39301065662705,
1.5707971514832),.UNSPECIFIED.) ;
#311 = B_SPLINE_CURVE_WITH_KNOTS('',3,(#10400,#10401,#10402,#10403,#10404,
#10405,#10406,#10407,#10408,#10409,#10410,#10411),.UNSPECIFIED.,.F.,.F.,
(4,2,2,2,2,4),(-0.0315121677712463,-0.0310393601655826,-0.0234386412048373,
-0.0156257279288386,-0.00781285405311264,0.),.UNSPECIFIED.) ;
#312 = B_SPLINE_CURVE_WITH_KNOTS('',3,(#10415,#10416,#10417,#10418,#10419,
#10420,#10421,#10422,#10423,#10424,#10425,#10426,#10427,#10428,#10429,#10430,
#10431,#10432,#10433,#10434,#10435,#10436,#10437,#10438,#10439),
 .UNSPECIFIED.,.F.,.F.,(4,3,3,3,3,3,3,3,4),(0.,0.199052542257445,0.39805950284863,
0.597027075005487,0.795961438919784,0.995008849693087,1.1939725966964,1.39300992521166,
1.57079632682576),.UNSPECIFIED.) ;
#313 = B_SPLINE_CURVE_WITH_KNOTS('',3,(#10445,#10446,#10447,#10448,#10449,
#10450,#10451,#10452,#10453,#10454,#10455,#10456),.UNSPECIFIED.,.F.,.F.,
(4,2,2,2,2,4),(-0.0315141739942469,-0.031204434348752,-0.0234384419466034,
-0.0156253478250137,-0.00781258702147206,0.),.UNSPECIFIED.) ;
#314 = B_SPLINE_CURVE_WITH_KNOTS('',3,(#10463,#10464,#10465,#10466,#10467,
#10468,#10469,#10470,#10471,#10472,#10473,#10474),.UNSPECIFIED.,.F.,.F.,
(4,2,2,2,2,4),(-0.0626970871191847,-0.0623734982158925,-0.054555633082751,
-0.0467389670549674,-0.0389250691737583,-0.0311774645911791),
 .UNSPECIFIED.) ;
#315 = B_SPLINE_CURVE_WITH_KNOTS('',3,(#10480,#10481,#10482,#10483,#10484,
#10485,#10486,#10487,#10488,#10489,#10490,#10491,#10492,#10493,#10494,#10495,
#10496,#10497,#10498,#10499,#10500,#10501,#10502,#10503,#10504),
 .UNSPECIFIED.,.F.,.F.,(4,3,3,3,3,3,3,3,4),(0.,0.199052686881998,0.398059792064997,
0.597027508785601,0.795962017240172,0.995009572636864,1.1939734642033,1.39301093733562,
1.57079746801826),.UNSPECIFIED.) ;
#316 = B_SPLINE_CURVE_WITH_KNOTS('',3,(#10510,#10511,#10512,#10513,#10514,
#10515,#10516,#10517,#10518,#10519,#10520,#10521),.UNSPECIFIED.,.F.,.F.,
(4,2,2,2,2,4),(-0.000404724526048245,0.,0.00770679420177707,0.015530569118343,
0.0233375581471532,0.0311349644051186),.UNSPECIFIED.) ;
#317 = B_SPLINE_CURVE_WITH_KNOTS('',3,(#10526,#10527,#10528,#10529,#10530,
#10531,#10532,#10533,#10534,#10535,#10536,#10537),.UNSPECIFIED.,.F.,.F.,
(4,2,2,2,2,4),(-0.0315136505422076,-0.0312114875916089,-0.0234386675146469,
-0.0156257772666477,-0.00781288830710044,0.),.UNSPECIFIED.) ;
#318 = B_SPLINE_CURVE_WITH_KNOTS('',3,(#10545,#10546,#10547,#10548,#10549,
#10550,#10551,#10552,#10553,#10554,#10555,#10556),.UNSPECIFIED.,.F.,.F.,
(4,2,2,2,2,4),(-0.0629751667751677,-0.0627714100781202,-0.0548037060202023,
-0.0469676168296412,-0.0391676281290893,-0.0313857050390938),
 .UNSPECIFIED.) ;
#319 = B_SPLINE_CURVE_WITH_KNOTS('',3,(#10560,#10561,#10562,#10563,#10564,
#10565,#10566,#10567,#10568,#10569,#10570,#10571),.UNSPECIFIED.,.F.,.F.,
(4,2,2,2,2,4),(-0.00020502755219765,0.,0.00797658615153273,0.015807888001696,
0.0236105688121075,0.031367048172),.UNSPECIFIED.) ;
#320 = B_SPLINE_CURVE_WITH_KNOTS('',3,(#10575,#10576,#10577,#10578,#10579,
#10580,#10581,#10582,#10583,#10584,#10585,#10586),.UNSPECIFIED.,.F.,.F.,
(4,2,2,2,2,4),(-0.0315146329369706,-0.0312183301295434,-0.0234383211620277,
-0.0156251214317014,-0.00781243022228811,0.),.UNSPECIFIED.) ;
#321 = B_SPLINE_CURVE_WITH_KNOTS('',3,(#10590,#10591,#10592,#10593,#10594,
#10595,#10596,#10597,#10598,#10599,#10600,#10601),.UNSPECIFIED.,.F.,.F.,
(4,2,2,2,2,4),(-0.00042586048217451,0.,0.00769137706195492,0.0155085087115375,
0.0233167456135432,0.0311209989547217),.UNSPECIFIED.) ;
#322 = B_SPLINE_CURVE_WITH_KNOTS('',3,(#10613,#10614,#10615,#10616,#10617,
#10618,#10619,#10620,#10621,#10622,#10623,#10624),.UNSPECIFIED.,.F.,.F.,
(4,2,2,2,2,4),(-0.0626464568378844,-0.0622205224951688,-0.0545426948140428,
-0.0467268743628218,-0.038917192768381,-0.0311102612475827),
 .UNSPECIFIED.) ;
#323 = B_SPLINE_CURVE_WITH_KNOTS('',3,(#10667,#10668,#10669,#10670,#10671,
#10672,#10673,#10674,#10675,#10676,#10677,#10678),.UNSPECIFIED.,.F.,.F.,
(4,2,2,2,2,4),(-0.000583318373026515,0.,0.00749040753634202,0.0153036497211779,
0.0231163526509165,0.0309287602356685),.UNSPECIFIED.) ;
#324 = B_SPLINE_CURVE_WITH_KNOTS('',3,(#10681,#10682,#10683,#10684,#10685,
#10686,#10687,#10688,#10689,#10690,#10691,#10692),.UNSPECIFIED.,.F.,.F.,
(4,2,2,2,2,4),(-0.0315120082952079,-0.0309286912237509,-0.0234383004008955,
-0.0156250756498918,-0.00781239015278319,0.),.UNSPECIFIED.) ;
#325 = B_SPLINE_CURVE_WITH_KNOTS('',3,(#10695,#10696,#10697,#10698,#10699,
#10700,#10701,#10702,#10703,#10704,#10705,#10706),.UNSPECIFIED.,.F.,.F.,
(4,2,2,2,2,4),(-0.0315120082952136,-0.0309286912237554,-0.0234383004008859,
-0.0156250756498869,-0.0078123901527818,0.),.UNSPECIFIED.) ;
#326 = B_SPLINE_CURVE_WITH_KNOTS('',3,(#10710,#10711,#10712,#10713,#10714,
#10715,#10716,#10717,#10718,#10719,#10720,#10721),.UNSPECIFIED.,.F.,.F.,
(4,2,2,2,2,4),(-0.000583318373025772,0.,0.0074904075363243,0.0153036497211384,
0.0231163526508542,0.0309287602355855),.UNSPECIFIED.) ;
#327 = B_SPLINE_CURVE_WITH_KNOTS('',3,(#10738,#10739,#10740,#10741,#10742,
#10743,#10744,#10745,#10746,#10747,#10748,#10749),.UNSPECIFIED.,.F.,.F.,
(4,2,2,2,2,4),(-0.030928760235604,-0.0231163526508699,-0.0153036497211549,
-0.00749040753633595,0.,0.000583318373037331),.UNSPECIFIED.) ;
#328 = B_SPLINE_CURVE_WITH_KNOTS('',3,(#10750,#10751,#10752,#10753,#10754,
#10755,#10756,#10757,#10758,#10759,#10760,#10761),.UNSPECIFIED.,.F.,.F.,
(4,2,2,2,2,4),(-0.0315120082952245,-0.0309286912237537,-0.0234383004008807,
-0.0156250756498813,-0.00781239015277872,0.),.UNSPECIFIED.) ;
#329 = B_SPLINE_CURVE_WITH_KNOTS('',3,(#10763,#10764,#10765,#10766,#10767,
#10768,#10769,#10770,#10771,#10772,#10773,#10774),.UNSPECIFIED.,.F.,.F.,
(4,2,2,2,2,4),(-0.0315120082952178,-0.0309286912237491,-0.0234383004008884,
-0.0156250756498874,-0.00781239015278138,0.),.UNSPECIFIED.) ;
#330 = B_SPLINE_CURVE_WITH_KNOTS('',3,(#10775,#10776,#10777,#10778,#10779,
#10780,#10781,#10782,#10783,#10784,#10785,#10786),.UNSPECIFIED.,.F.,.F.,
(4,2,2,2,2,4),(-0.00058331837303795,0.,0.00749040753635054,0.0153036497211894,
0.0231163526509301,0.0309287602356871),.UNSPECIFIED.) ;
#331 = B_SPLINE_CURVE_WITH_KNOTS('',3,(#10992,#10993,#10994,#10995,#10996,
#10997,#10998,#10999,#11000,#11001,#11002,#11003,#11004,#11005),
 .UNSPECIFIED.,.F.,.F.,(4,2,2,2,2,2,4),(-0.0259307736234173,-0.0249485644999998,
-0.0216439933226257,-0.0192686778677155,-0.0180929024728077,-0.0172645332734243,
-0.0172587275311834),.UNSPECIFIED.) ;
#332 = B_SPLINE_CURVE_WITH_KNOTS('',3,(#11007,#11008,#11009,#11010,#11011,
#11012,#11013,#11014,#11015,#11016,#11017,#11018,#11019,#11020,#11021,#11022,
#11023,#11024,#11025,#11026,#11027,#11028,#11029,#11030,#11031,#11032,#11033,
#11034),.UNSPECIFIED.,.F.,.F.,(4,2,2,2,2,2,2,2,2,2,2,2,2,4),(-0.227861047738708,
-0.227391834147561,-0.205936841126713,-0.182802806411279,-0.158511575631131,
-0.139726830403032,-0.124097041482524,-0.113695917073779,-0.103294792665033,
-0.0876650037445263,-0.0688802585164366,-0.0445890277362838,-0.0214549930208493,
-0.0104677835050617),.UNSPECIFIED.) ;
#333 = B_SPLINE_CURVE_WITH_KNOTS('',3,(#11036,#11037,#11038,#11039,#11040,
#11041,#11042,#11043,#11044,#11045,#11046,#11047,#11048,#11049,#11050,#11051,
#11052,#11053,#11054,#11055,#11056,#11057,#11058,#11059,#11060,#11061,#11062,
#11063),.UNSPECIFIED.,.F.,.F.,(4,2,2,2,2,2,2,2,2,2,2,2,2,4),(-0.216924050647861,
-0.205936841131769,-0.18280280641576,-0.158511575635004,-0.139726830406447,
-0.124097041485557,-0.11369591707655,-0.103294792667543,-0.0876650037466527,
-0.0688802585180876,-0.0445890277373239,-0.0214549930213075,0.,0.000469213591169131),
 .UNSPECIFIED.) ;
#334 = B_SPLINE_CURVE_WITH_KNOTS('',3,(#11064,#11065,#11066,#11067,#11068,
#11069,#11070,#11071,#11072,#11073,#11074,#11075),.UNSPECIFIED.,.F.,.F.,
(4,2,2,2,2,4),(-0.0172587275311834,-0.0164381703856616,-0.0152719978296815,
-0.0126858911745641,-0.00874619308042844,-0.00858294775784745),
 .UNSPECIFIED.) ;
#335 = B_SPLINE_CURVE_WITH_KNOTS('',3,(#11092,#11093,#11094,#11095,#11096,
#11097,#11098,#11099,#11100,#11101,#11102,#11103,#11104,#11105,#11106,#11107,
#11108,#11109,#11110,#11111,#11112,#11113,#11114,#11115,#11116,#11117,#11118,
#11119),.UNSPECIFIED.,.F.,.F.,(4,2,2,2,2,2,2,2,2,2,2,2,2,4),(-0.395561282223792,
-0.371589813708337,-0.344453097699251,-0.238518055903461,-0.203039163893727,
-0.181087404891762,-0.170436776518923,-0.161871312257026,-0.152337951045022,
-0.140457204945395,-0.136918737460203,-0.135513383219719,-0.13466047941831,
-0.134248321319432),.UNSPECIFIED.) ;
#336 = B_SPLINE_CURVE_WITH_KNOTS('',3,(#11126,#11127,#11128,#11129,#11130,
#11131,#11132,#11133,#11134,#11135,#11136,#11137,#11138,#11139,#11140,#11141,
#11142,#11143,#11144,#11145,#11146,#11147,#11148,#11149,#11150,#11151),
 .UNSPECIFIED.,.F.,.F.,(4,2,2,2,2,2,2,2,2,2,2,2,4),(-1.12946917222019,-0.956778050613223,
-0.699790449652219,-0.624100552674695,-0.590735740809338,-0.565825455088631,
-0.541939131211673,-0.511943639238009,-0.463169452478806,-0.380157846166964,
-0.241539556580725,0.,0.0019944793498423),.UNSPECIFIED.) ;
#337 = FACE_BOUND('',#849,.T.) ;
#338 = FACE_BOUND('',#853,.T.) ;
#339 = FACE_BOUND('',#856,.T.) ;
#340 = FACE_BOUND('',#867,.T.) ;
#341 = FACE_BOUND('',#868,.T.) ;
#342 = FACE_BOUND('',#873,.T.) ;
#343 = FACE_BOUND('',#874,.T.) ;
#344 = FACE_BOUND('',#906,.T.) ;
#345 = FACE_BOUND('',#912,.T.) ;
#346 = FACE_BOUND('',#926,.T.) ;
#347 = FACE_BOUND('',#942,.T.) ;
#348 = FACE_BOUND('',#943,.T.) ;
#349 = FACE_BOUND('',#944,.T.) ;
#350 = FACE_BOUND('',#945,.T.) ;
#351 = FACE_BOUND('',#949,.T.) ;
#352 = FACE_BOUND('',#953,.T.) ;
#353 = FACE_BOUND('',#961,.T.) ;
#354 = FACE_BOUND('',#962,.T.) ;
#355 = FACE_BOUND('',#992,.T.) ;
#356 = FACE_BOUND('',#998,.T.) ;
#357 = FACE_BOUND('',#1000,.T.) ;
#358 = FACE_BOUND('',#1001,.T.) ;
#359 = FACE_BOUND('',#1053,.T.) ;
#360 = FACE_BOUND('',#1054,.T.) ;
#361 = FACE_BOUND('',#1099,.T.) ;
#362 = FACE_BOUND('',#1100,.T.) ;
#363 = FACE_BOUND('',#1122,.T.) ;
#364 = FACE_BOUND('',#1127,.T.) ;
#365 = FACE_BOUND('',#1146,.T.) ;
#366 = FACE_BOUND('',#1148,.T.) ;
#367 = FACE_BOUND('',#1157,.T.) ;
#368 = FACE_BOUND('',#1174,.T.) ;
#369 = FACE_BOUND('',#1177,.T.) ;
#370 = FACE_BOUND('',#1180,.T.) ;
#371 = FACE_BOUND('',#1183,.T.) ;
#372 = FACE_BOUND('',#1186,.T.) ;
#373 = FACE_BOUND('',#1189,.T.) ;
#374 = FACE_BOUND('',#1212,.T.) ;
#375 = FACE_BOUND('',#1214,.T.) ;
#376 = FACE_BOUND('',#1217,.T.) ;
#377 = FACE_BOUND('',#1220,.T.) ;
#378 = ELLIPSE('',#5762,4.97501164804779,3.175) ;
#379 = ELLIPSE('',#5763,4.97501164804779,3.175) ;
#380 = ELLIPSE('',#5772,4.72548959035073,3.175) ;
#381 = ELLIPSE('',#5773,3.9949536559852,3.175) ;
#382 = ELLIPSE('',#5774,3.37510195454879,3.175) ;
#383 = ELLIPSE('',#5826,3.79929660772484,2.925) ;
#384 = ELLIPSE('',#5866,3.9949536559852,3.175) ;
#385 = ELLIPSE('',#5867,3.79929660772485,2.925) ;
#386 = ELLIPSE('',#5875,1.79605122421383,1.27) ;
#387 = ELLIPSE('',#5878,1.79605122421383,1.27) ;
#388 = ELLIPSE('',#5883,3.37510195454879,3.175) ;
#389 = ELLIPSE('',#5884,4.72548959035073,3.175) ;
#390 = ELLIPSE('',#5889,3.3147973165791,3.175) ;
#391 = ELLIPSE('',#5897,3.3147973165791,3.175) ;
#392 = ELLIPSE('',#5926,0.353553390593277,0.25) ;
#393 = ELLIPSE('',#5939,0.353553390593277,0.25) ;
#394 = ELLIPSE('',#6060,0.200007949139568,0.2) ;
#395 = ELLIPSE('',#6150,0.200007949139572,0.2) ;
#396 = PLANE('',#5761) ;
#397 = PLANE('',#5764) ;
#398 = PLANE('',#5765) ;
#399 = PLANE('',#5766) ;
#400 = PLANE('',#5767) ;
#401 = PLANE('',#5768) ;
#402 = PLANE('',#5769) ;
#403 = PLANE('',#5770) ;
#404 = PLANE('',#5775) ;
#405 = PLANE('',#5788) ;
#406 = PLANE('',#5791) ;
#407 = PLANE('',#5806) ;
#408 = PLANE('',#5823) ;
#409 = PLANE('',#5872) ;
#410 = PLANE('',#5876) ;
#411 = PLANE('',#5880) ;
#412 = PLANE('',#5890) ;
#413 = PLANE('',#5891) ;
#414 = PLANE('',#5894) ;
#415 = PLANE('',#5900) ;
#416 = PLANE('',#5901) ;
#417 = PLANE('',#5904) ;
#418 = PLANE('',#5907) ;
#419 = PLANE('',#5910) ;
#420 = PLANE('',#5913) ;
#421 = PLANE('',#5916) ;
#422 = PLANE('',#5919) ;
#423 = PLANE('',#5922) ;
#424 = PLANE('',#5930) ;
#425 = PLANE('',#5940) ;
#426 = PLANE('',#5956) ;
#427 = PLANE('',#5959) ;
#428 = PLANE('',#5977) ;
#429 = PLANE('',#6001) ;
#430 = PLANE('',#6004) ;
#431 = PLANE('',#6011) ;
#432 = PLANE('',#6014) ;
#433 = PLANE('',#6019) ;
#434 = PLANE('',#6022) ;
#435 = PLANE('',#6023) ;
#436 = PLANE('',#6026) ;
#437 = PLANE('',#6027) ;
#438 = PLANE('',#6029) ;
#439 = PLANE('',#6032) ;
#440 = PLANE('',#6034) ;
#441 = PLANE('',#6036) ;
#442 = PLANE('',#6102) ;
#443 = PLANE('',#6105) ;
#444 = PLANE('',#6108) ;
#445 = PLANE('',#6113) ;
#446 = PLANE('',#6116) ;
#447 = PLANE('',#6121) ;
#448 = PLANE('',#6124) ;
#449 = PLANE('',#6180) ;
#450 = PLANE('',#6182) ;
#451 = PLANE('',#6184) ;
#452 = PLANE('',#6186) ;
#453 = PLANE('',#6188) ;
#454 = PLANE('',#6190) ;
#455 = PLANE('',#6191) ;
#456 = PLANE('',#6193) ;
#457 = PLANE('',#6194) ;
#458 = PLANE('',#6206) ;
#459 = PLANE('',#6213) ;
#460 = PLANE('',#6216) ;
#461 = PLANE('',#6224) ;
#462 = PLANE('',#6226) ;
#463 = PLANE('',#6230) ;
#464 = PLANE('',#6238) ;
#465 = PLANE('',#6242) ;
#466 = PLANE('',#6244) ;
#467 = PLANE('',#6252) ;
#468 = PLANE('',#6257) ;
#469 = PLANE('',#6258) ;
#470 = PLANE('',#6259) ;
#471 = PLANE('',#6260) ;
#472 = PLANE('',#6261) ;
#473 = PLANE('',#6262) ;
#474 = PLANE('',#6263) ;
#475 = PLANE('',#6264) ;
#476 = PLANE('',#6265) ;
#477 = PLANE('',#6266) ;
#478 = PLANE('',#6267) ;
#479 = PLANE('',#6269) ;
#480 = PLANE('',#6270) ;
#481 = PLANE('',#6271) ;
#482 = PLANE('',#6272) ;
#483 = PLANE('',#6273) ;
#484 = PLANE('',#6274) ;
#485 = PLANE('',#6275) ;
#486 = PLANE('',#6276) ;
#487 = PLANE('',#6288) ;
#488 = PLANE('',#6315) ;
#489 = PLANE('',#6319) ;
#490 = PLANE('',#6324) ;
#491 = PLANE('',#6328) ;
#492 = PLANE('',#6333) ;
#493 = PLANE('',#6337) ;
#494 = PLANE('',#6342) ;
#495 = PLANE('',#6343) ;
#496 = PLANE('',#6347) ;
#497 = PLANE('',#6354) ;
#498 = PLANE('',#6355) ;
#499 = PLANE('',#6356) ;
#500 = PLANE('',#6364) ;
#501 = PLANE('',#6371) ;
#502 = PLANE('',#6375) ;
#503 = PLANE('',#6382) ;
#504 = PLANE('',#6383) ;
#505 = PLANE('',#6384) ;
#506 = PLANE('',#6389) ;
#507 = PLANE('',#6393) ;
#508 = FACE_OUTER_BOUND('',#844,.T.) ;
#509 = FACE_OUTER_BOUND('',#845,.T.) ;
#510 = FACE_OUTER_BOUND('',#846,.T.) ;
#511 = FACE_OUTER_BOUND('',#847,.T.) ;
#512 = FACE_OUTER_BOUND('',#848,.T.) ;
#513 = FACE_OUTER_BOUND('',#850,.T.) ;
#514 = FACE_OUTER_BOUND('',#851,.T.) ;
#515 = FACE_OUTER_BOUND('',#852,.T.) ;
#516 = FACE_OUTER_BOUND('',#854,.T.) ;
#517 = FACE_OUTER_BOUND('',#855,.T.) ;
#518 = FACE_OUTER_BOUND('',#857,.T.) ;
#519 = FACE_OUTER_BOUND('',#858,.T.) ;
#520 = FACE_OUTER_BOUND('',#859,.T.) ;
#521 = FACE_OUTER_BOUND('',#860,.T.) ;
#522 = FACE_OUTER_BOUND('',#861,.T.) ;
#523 = FACE_OUTER_BOUND('',#862,.T.) ;
#524 = FACE_OUTER_BOUND('',#863,.T.) ;
#525 = FACE_OUTER_BOUND('',#864,.T.) ;
#526 = FACE_OUTER_BOUND('',#865,.T.) ;
#527 = FACE_OUTER_BOUND('',#866,.T.) ;
#528 = FACE_OUTER_BOUND('',#869,.T.) ;
#529 = FACE_OUTER_BOUND('',#870,.T.) ;
#530 = FACE_OUTER_BOUND('',#871,.T.) ;
#531 = FACE_OUTER_BOUND('',#872,.T.) ;
#532 = FACE_OUTER_BOUND('',#875,.T.) ;
#533 = FACE_OUTER_BOUND('',#876,.T.) ;
#534 = FACE_OUTER_BOUND('',#877,.T.) ;
#535 = FACE_OUTER_BOUND('',#878,.T.) ;
#536 = FACE_OUTER_BOUND('',#879,.T.) ;
#537 = FACE_OUTER_BOUND('',#880,.T.) ;
#538 = FACE_OUTER_BOUND('',#881,.T.) ;
#539 = FACE_OUTER_BOUND('',#882,.T.) ;
#540 = FACE_OUTER_BOUND('',#883,.T.) ;
#541 = FACE_OUTER_BOUND('',#884,.T.) ;
#542 = FACE_OUTER_BOUND('',#885,.T.) ;
#543 = FACE_OUTER_BOUND('',#886,.T.) ;
#544 = FACE_OUTER_BOUND('',#887,.T.) ;
#545 = FACE_OUTER_BOUND('',#888,.T.) ;
#546 = FACE_OUTER_BOUND('',#889,.T.) ;
#547 = FACE_OUTER_BOUND('',#890,.T.) ;
#548 = FACE_OUTER_BOUND('',#891,.T.) ;
#549 = FACE_OUTER_BOUND('',#892,.T.) ;
#550 = FACE_OUTER_BOUND('',#893,.T.) ;
#551 = FACE_OUTER_BOUND('',#894,.T.) ;
#552 = FACE_OUTER_BOUND('',#895,.T.) ;
#553 = FACE_OUTER_BOUND('',#896,.T.) ;
#554 = FACE_OUTER_BOUND('',#897,.T.) ;
#555 = FACE_OUTER_BOUND('',#898,.T.) ;
#556 = FACE_OUTER_BOUND('',#899,.T.) ;
#557 = FACE_OUTER_BOUND('',#900,.T.) ;
#558 = FACE_OUTER_BOUND('',#901,.T.) ;
#559 = FACE_OUTER_BOUND('',#902,.T.) ;
#560 = FACE_OUTER_BOUND('',#903,.T.) ;
#561 = FACE_OUTER_BOUND('',#904,.T.) ;
#562 = FACE_OUTER_BOUND('',#905,.T.) ;
#563 = FACE_OUTER_BOUND('',#907,.T.) ;
#564 = FACE_OUTER_BOUND('',#908,.T.) ;
#565 = FACE_OUTER_BOUND('',#909,.T.) ;
#566 = FACE_OUTER_BOUND('',#910,.T.) ;
#567 = FACE_OUTER_BOUND('',#911,.T.) ;
#568 = FACE_OUTER_BOUND('',#913,.T.) ;
#569 = FACE_OUTER_BOUND('',#914,.T.) ;
#570 = FACE_OUTER_BOUND('',#915,.T.) ;
#571 = FACE_OUTER_BOUND('',#916,.T.) ;
#572 = FACE_OUTER_BOUND('',#917,.T.) ;
#573 = FACE_OUTER_BOUND('',#918,.T.) ;
#574 = FACE_OUTER_BOUND('',#919,.T.) ;
#575 = FACE_OUTER_BOUND('',#920,.T.) ;
#576 = FACE_OUTER_BOUND('',#921,.T.) ;
#577 = FACE_OUTER_BOUND('',#922,.T.) ;
#578 = FACE_OUTER_BOUND('',#923,.T.) ;
#579 = FACE_OUTER_BOUND('',#924,.T.) ;
#580 = FACE_OUTER_BOUND('',#925,.T.) ;
#581 = FACE_OUTER_BOUND('',#927,.T.) ;
#582 = FACE_OUTER_BOUND('',#928,.T.) ;
#583 = FACE_OUTER_BOUND('',#929,.T.) ;
#584 = FACE_OUTER_BOUND('',#930,.T.) ;
#585 = FACE_OUTER_BOUND('',#931,.T.) ;
#586 = FACE_OUTER_BOUND('',#932,.T.) ;
#587 = FACE_OUTER_BOUND('',#933,.T.) ;
#588 = FACE_OUTER_BOUND('',#934,.T.) ;
#589 = FACE_OUTER_BOUND('',#935,.T.) ;
#590 = FACE_OUTER_BOUND('',#936,.T.) ;
#591 = FACE_OUTER_BOUND('',#937,.T.) ;
#592 = FACE_OUTER_BOUND('',#938,.T.) ;
#593 = FACE_OUTER_BOUND('',#939,.T.) ;
#594 = FACE_OUTER_BOUND('',#940,.T.) ;
#595 = FACE_OUTER_BOUND('',#941,.T.) ;
#596 = FACE_OUTER_BOUND('',#946,.T.) ;
#597 = FACE_OUTER_BOUND('',#947,.T.) ;
#598 = FACE_OUTER_BOUND('',#948,.T.) ;
#599 = FACE_OUTER_BOUND('',#950,.T.) ;
#600 = FACE_OUTER_BOUND('',#951,.T.) ;
#601 = FACE_OUTER_BOUND('',#952,.T.) ;
#602 = FACE_OUTER_BOUND('',#954,.T.) ;
#603 = FACE_OUTER_BOUND('',#955,.T.) ;
#604 = FACE_OUTER_BOUND('',#956,.T.) ;
#605 = FACE_OUTER_BOUND('',#957,.T.) ;
#606 = FACE_OUTER_BOUND('',#958,.T.) ;
#607 = FACE_OUTER_BOUND('',#959,.T.) ;
#608 = FACE_OUTER_BOUND('',#960,.T.) ;
#609 = FACE_OUTER_BOUND('',#963,.T.) ;
#610 = FACE_OUTER_BOUND('',#964,.T.) ;
#611 = FACE_OUTER_BOUND('',#965,.T.) ;
#612 = FACE_OUTER_BOUND('',#966,.T.) ;
#613 = FACE_OUTER_BOUND('',#967,.T.) ;
#614 = FACE_OUTER_BOUND('',#968,.T.) ;
#615 = FACE_OUTER_BOUND('',#969,.T.) ;
#616 = FACE_OUTER_BOUND('',#970,.T.) ;
#617 = FACE_OUTER_BOUND('',#971,.T.) ;
#618 = FACE_OUTER_BOUND('',#972,.T.) ;
#619 = FACE_OUTER_BOUND('',#973,.T.) ;
#620 = FACE_OUTER_BOUND('',#974,.T.) ;
#621 = FACE_OUTER_BOUND('',#975,.T.) ;
#622 = FACE_OUTER_BOUND('',#976,.T.) ;
#623 = FACE_OUTER_BOUND('',#977,.T.) ;
#624 = FACE_OUTER_BOUND('',#978,.T.) ;
#625 = FACE_OUTER_BOUND('',#979,.T.) ;
#626 = FACE_OUTER_BOUND('',#980,.T.) ;
#627 = FACE_OUTER_BOUND('',#981,.T.) ;
#628 = FACE_OUTER_BOUND('',#982,.T.) ;
#629 = FACE_OUTER_BOUND('',#983,.T.) ;
#630 = FACE_OUTER_BOUND('',#984,.T.) ;
#631 = FACE_OUTER_BOUND('',#985,.T.) ;
#632 = FACE_OUTER_BOUND('',#986,.T.) ;
#633 = FACE_OUTER_BOUND('',#987,.T.) ;
#634 = FACE_OUTER_BOUND('',#988,.T.) ;
#635 = FACE_OUTER_BOUND('',#989,.T.) ;
#636 = FACE_OUTER_BOUND('',#990,.T.) ;
#637 = FACE_OUTER_BOUND('',#991,.T.) ;
#638 = FACE_OUTER_BOUND('',#993,.T.) ;
#639 = FACE_OUTER_BOUND('',#994,.T.) ;
#640 = FACE_OUTER_BOUND('',#995,.T.) ;
#641 = FACE_OUTER_BOUND('',#996,.T.) ;
#642 = FACE_OUTER_BOUND('',#997,.T.) ;
#643 = FACE_OUTER_BOUND('',#999,.T.) ;
#644 = FACE_OUTER_BOUND('',#1002,.T.) ;
#645 = FACE_OUTER_BOUND('',#1003,.T.) ;
#646 = FACE_OUTER_BOUND('',#1004,.T.) ;
#647 = FACE_OUTER_BOUND('',#1005,.T.) ;
#648 = FACE_OUTER_BOUND('',#1006,.T.) ;
#649 = FACE_OUTER_BOUND('',#1007,.T.) ;
#650 = FACE_OUTER_BOUND('',#1008,.T.) ;
#651 = FACE_OUTER_BOUND('',#1009,.T.) ;
#652 = FACE_OUTER_BOUND('',#1010,.T.) ;
#653 = FACE_OUTER_BOUND('',#1011,.T.) ;
#654 = FACE_OUTER_BOUND('',#1012,.T.) ;
#655 = FACE_OUTER_BOUND('',#1013,.T.) ;
#656 = FACE_OUTER_BOUND('',#1014,.T.) ;
#657 = FACE_OUTER_BOUND('',#1015,.T.) ;
#658 = FACE_OUTER_BOUND('',#1016,.T.) ;
#659 = FACE_OUTER_BOUND('',#1017,.T.) ;
#660 = FACE_OUTER_BOUND('',#1018,.T.) ;
#661 = FACE_OUTER_BOUND('',#1019,.T.) ;
#662 = FACE_OUTER_BOUND('',#1020,.T.) ;
#663 = FACE_OUTER_BOUND('',#1021,.T.) ;
#664 = FACE_OUTER_BOUND('',#1022,.T.) ;
#665 = FACE_OUTER_BOUND('',#1023,.T.) ;
#666 = FACE_OUTER_BOUND('',#1024,.T.) ;
#667 = FACE_OUTER_BOUND('',#1025,.T.) ;
#668 = FACE_OUTER_BOUND('',#1026,.T.) ;
#669 = FACE_OUTER_BOUND('',#1027,.T.) ;
#670 = FACE_OUTER_BOUND('',#1028,.T.) ;
#671 = FACE_OUTER_BOUND('',#1029,.T.) ;
#672 = FACE_OUTER_BOUND('',#1030,.T.) ;
#673 = FACE_OUTER_BOUND('',#1031,.T.) ;
#674 = FACE_OUTER_BOUND('',#1032,.T.) ;
#675 = FACE_OUTER_BOUND('',#1033,.T.) ;
#676 = FACE_OUTER_BOUND('',#1034,.T.) ;
#677 = FACE_OUTER_BOUND('',#1035,.T.) ;
#678 = FACE_OUTER_BOUND('',#1036,.T.) ;
#679 = FACE_OUTER_BOUND('',#1037,.T.) ;
#680 = FACE_OUTER_BOUND('',#1038,.T.) ;
#681 = FACE_OUTER_BOUND('',#1039,.T.) ;
#682 = FACE_OUTER_BOUND('',#1040,.T.) ;
#683 = FACE_OUTER_BOUND('',#1041,.T.) ;
#684 = FACE_OUTER_BOUND('',#1042,.T.) ;
#685 = FACE_OUTER_BOUND('',#1043,.T.) ;
#686 = FACE_OUTER_BOUND('',#1044,.T.) ;
#687 = FACE_OUTER_BOUND('',#1045,.T.) ;
#688 = FACE_OUTER_BOUND('',#1046,.T.) ;
#689 = FACE_OUTER_BOUND('',#1047,.T.) ;
#690 = FACE_OUTER_BOUND('',#1048,.T.) ;
#691 = FACE_OUTER_BOUND('',#1049,.T.) ;
#692 = FACE_OUTER_BOUND('',#1050,.T.) ;
#693 = FACE_OUTER_BOUND('',#1051,.T.) ;
#694 = FACE_OUTER_BOUND('',#1052,.T.) ;
#695 = FACE_OUTER_BOUND('',#1055,.T.) ;
#696 = FACE_OUTER_BOUND('',#1056,.T.) ;
#697 = FACE_OUTER_BOUND('',#1057,.T.) ;
#698 = FACE_OUTER_BOUND('',#1058,.T.) ;
#699 = FACE_OUTER_BOUND('',#1059,.T.) ;
#700 = FACE_OUTER_BOUND('',#1060,.T.) ;
#701 = FACE_OUTER_BOUND('',#1061,.T.) ;
#702 = FACE_OUTER_BOUND('',#1062,.T.) ;
#703 = FACE_OUTER_BOUND('',#1063,.T.) ;
#704 = FACE_OUTER_BOUND('',#1064,.T.) ;
#705 = FACE_OUTER_BOUND('',#1065,.T.) ;
#706 = FACE_OUTER_BOUND('',#1066,.T.) ;
#707 = FACE_OUTER_BOUND('',#1067,.T.) ;
#708 = FACE_OUTER_BOUND('',#1068,.T.) ;
#709 = FACE_OUTER_BOUND('',#1069,.T.) ;
#710 = FACE_OUTER_BOUND('',#1070,.T.) ;
#711 = FACE_OUTER_BOUND('',#1071,.T.) ;
#712 = FACE_OUTER_BOUND('',#1072,.T.) ;
#713 = FACE_OUTER_BOUND('',#1073,.T.) ;
#714 = FACE_OUTER_BOUND('',#1074,.T.) ;
#715 = FACE_OUTER_BOUND('',#1075,.T.) ;
#716 = FACE_OUTER_BOUND('',#1076,.T.) ;
#717 = FACE_OUTER_BOUND('',#1077,.T.) ;
#718 = FACE_OUTER_BOUND('',#1078,.T.) ;
#719 = FACE_OUTER_BOUND('',#1079,.T.) ;
#720 = FACE_OUTER_BOUND('',#1080,.T.) ;
#721 = FACE_OUTER_BOUND('',#1081,.T.) ;
#722 = FACE_OUTER_BOUND('',#1082,.T.) ;
#723 = FACE_OUTER_BOUND('',#1083,.T.) ;
#724 = FACE_OUTER_BOUND('',#1084,.T.) ;
#725 = FACE_OUTER_BOUND('',#1085,.T.) ;
#726 = FACE_OUTER_BOUND('',#1086,.T.) ;
#727 = FACE_OUTER_BOUND('',#1087,.T.) ;
#728 = FACE_OUTER_BOUND('',#1088,.T.) ;
#729 = FACE_OUTER_BOUND('',#1089,.T.) ;
#730 = FACE_OUTER_BOUND('',#1090,.T.) ;
#731 = FACE_OUTER_BOUND('',#1091,.T.) ;
#732 = FACE_OUTER_BOUND('',#1092,.T.) ;
#733 = FACE_OUTER_BOUND('',#1093,.T.) ;
#734 = FACE_OUTER_BOUND('',#1094,.T.) ;
#735 = FACE_OUTER_BOUND('',#1095,.T.) ;
#736 = FACE_OUTER_BOUND('',#1096,.T.) ;
#737 = FACE_OUTER_BOUND('',#1097,.T.) ;
#738 = FACE_OUTER_BOUND('',#1098,.T.) ;
#739 = FACE_OUTER_BOUND('',#1101,.T.) ;
#740 = FACE_OUTER_BOUND('',#1102,.T.) ;
#741 = FACE_OUTER_BOUND('',#1103,.T.) ;
#742 = FACE_OUTER_BOUND('',#1104,.T.) ;
#743 = FACE_OUTER_BOUND('',#1105,.T.) ;
#744 = FACE_OUTER_BOUND('',#1106,.T.) ;
#745 = FACE_OUTER_BOUND('',#1107,.T.) ;
#746 = FACE_OUTER_BOUND('',#1108,.T.) ;
#747 = FACE_OUTER_BOUND('',#1109,.T.) ;
#748 = FACE_OUTER_BOUND('',#1110,.T.) ;
#749 = FACE_OUTER_BOUND('',#1111,.T.) ;
#750 = FACE_OUTER_BOUND('',#1112,.T.) ;
#751 = FACE_OUTER_BOUND('',#1113,.T.) ;
#752 = FACE_OUTER_BOUND('',#1114,.T.) ;
#753 = FACE_OUTER_BOUND('',#1115,.T.) ;
#754 = FACE_OUTER_BOUND('',#1116,.T.) ;
#755 = FACE_OUTER_BOUND('',#1117,.T.) ;
#756 = FACE_OUTER_BOUND('',#1118,.T.) ;
#757 = FACE_OUTER_BOUND('',#1119,.T.) ;
#758 = FACE_OUTER_BOUND('',#1120,.T.) ;
#759 = FACE_OUTER_BOUND('',#1121,.T.) ;
#760 = FACE_OUTER_BOUND('',#1123,.T.) ;
#761 = FACE_OUTER_BOUND('',#1124,.T.) ;
#762 = FACE_OUTER_BOUND('',#1125,.T.) ;
#763 = FACE_OUTER_BOUND('',#1126,.T.) ;
#764 = FACE_OUTER_BOUND('',#1128,.T.) ;
#765 = FACE_OUTER_BOUND('',#1129,.T.) ;
#766 = FACE_OUTER_BOUND('',#1130,.T.) ;
#767 = FACE_OUTER_BOUND('',#1131,.T.) ;
#768 = FACE_OUTER_BOUND('',#1132,.T.) ;
#769 = FACE_OUTER_BOUND('',#1133,.T.) ;
#770 = FACE_OUTER_BOUND('',#1134,.T.) ;
#771 = FACE_OUTER_BOUND('',#1135,.T.) ;
#772 = FACE_OUTER_BOUND('',#1136,.T.) ;
#773 = FACE_OUTER_BOUND('',#1137,.T.) ;
#774 = FACE_OUTER_BOUND('',#1138,.T.) ;
#775 = FACE_OUTER_BOUND('',#1139,.T.) ;
#776 = FACE_OUTER_BOUND('',#1140,.T.) ;
#777 = FACE_OUTER_BOUND('',#1141,.T.) ;
#778 = FACE_OUTER_BOUND('',#1142,.T.) ;
#779 = FACE_OUTER_BOUND('',#1143,.T.) ;
#780 = FACE_OUTER_BOUND('',#1144,.T.) ;
#781 = FACE_OUTER_BOUND('',#1145,.T.) ;
#782 = FACE_OUTER_BOUND('',#1147,.T.) ;
#783 = FACE_OUTER_BOUND('',#1149,.T.) ;
#784 = FACE_OUTER_BOUND('',#1150,.T.) ;
#785 = FACE_OUTER_BOUND('',#1151,.T.) ;
#786 = FACE_OUTER_BOUND('',#1152,.T.) ;
#787 = FACE_OUTER_BOUND('',#1153,.T.) ;
#788 = FACE_OUTER_BOUND('',#1154,.T.) ;
#789 = FACE_OUTER_BOUND('',#1155,.T.) ;
#790 = FACE_OUTER_BOUND('',#1156,.T.) ;
#791 = FACE_OUTER_BOUND('',#1158,.T.) ;
#792 = FACE_OUTER_BOUND('',#1159,.T.) ;
#793 = FACE_OUTER_BOUND('',#1160,.T.) ;
#794 = FACE_OUTER_BOUND('',#1161,.T.) ;
#795 = FACE_OUTER_BOUND('',#1162,.T.) ;
#796 = FACE_OUTER_BOUND('',#1163,.T.) ;
#797 = FACE_OUTER_BOUND('',#1164,.T.) ;
#798 = FACE_OUTER_BOUND('',#1165,.T.) ;
#799 = FACE_OUTER_BOUND('',#1166,.T.) ;
#800 = FACE_OUTER_BOUND('',#1167,.T.) ;
#801 = FACE_OUTER_BOUND('',#1168,.T.) ;
#802 = FACE_OUTER_BOUND('',#1169,.T.) ;
#803 = FACE_OUTER_BOUND('',#1170,.T.) ;
#804 = FACE_OUTER_BOUND('',#1171,.T.) ;
#805 = FACE_OUTER_BOUND('',#1172,.T.) ;
#806 = FACE_OUTER_BOUND('',#1173,.T.) ;
#807 = FACE_OUTER_BOUND('',#1175,.T.) ;
#808 = FACE_OUTER_BOUND('',#1176,.T.) ;
#809 = FACE_OUTER_BOUND('',#1178,.T.) ;
#810 = FACE_OUTER_BOUND('',#1179,.T.) ;
#811 = FACE_OUTER_BOUND('',#1181,.T.) ;
#812 = FACE_OUTER_BOUND('',#1182,.T.) ;
#813 = FACE_OUTER_BOUND('',#1184,.T.) ;
#814 = FACE_OUTER_BOUND('',#1185,.T.) ;
#815 = FACE_OUTER_BOUND('',#1187,.T.) ;
#816 = FACE_OUTER_BOUND('',#1188,.T.) ;
#817 = FACE_OUTER_BOUND('',#1190,.T.) ;
#818 = FACE_OUTER_BOUND('',#1191,.T.) ;
#819 = FACE_OUTER_BOUND('',#1192,.T.) ;
#820 = FACE_OUTER_BOUND('',#1193,.T.) ;
#821 = FACE_OUTER_BOUND('',#1194,.T.) ;
#822 = FACE_OUTER_BOUND('',#1195,.T.) ;
#823 = FACE_OUTER_BOUND('',#1196,.T.) ;
#824 = FACE_OUTER_BOUND('',#1197,.T.) ;
#825 = FACE_OUTER_BOUND('',#1198,.T.) ;
#826 = FACE_OUTER_BOUND('',#1199,.T.) ;
#827 = FACE_OUTER_BOUND('',#1200,.T.) ;
#828 = FACE_OUTER_BOUND('',#1201,.T.) ;
#829 = FACE_OUTER_BOUND('',#1202,.T.) ;
#830 = FACE_OUTER_BOUND('',#1203,.T.) ;
#831 = FACE_OUTER_BOUND('',#1204,.T.) ;
#832 = FACE_OUTER_BOUND('',#1205,.T.) ;
#833 = FACE_OUTER_BOUND('',#1206,.T.) ;
#834 = FACE_OUTER_BOUND('',#1207,.T.) ;
#835 = FACE_OUTER_BOUND('',#1208,.T.) ;
#836 = FACE_OUTER_BOUND('',#1209,.T.) ;
#837 = FACE_OUTER_BOUND('',#1210,.T.) ;
#838 = FACE_OUTER_BOUND('',#1211,.T.) ;
#839 = FACE_OUTER_BOUND('',#1213,.T.) ;
#840 = FACE_OUTER_BOUND('',#1215,.T.) ;
#841 = FACE_OUTER_BOUND('',#1216,.T.) ;
#842 = FACE_OUTER_BOUND('',#1218,.T.) ;
#843 = FACE_OUTER_BOUND('',#1219,.T.) ;
#844 = EDGE_LOOP('',(#3528,#3529,#3530,#3531)) ;
#845 = EDGE_LOOP('',(#3532,#3533,#3534,#3535)) ;
#846 = EDGE_LOOP('',(#3536,#3537,#3538,#3539)) ;
#847 = EDGE_LOOP('',(#3540,#3541,#3542,#3543,#3544,#3545)) ;
#848 = EDGE_LOOP('',(#3546,#3547,#3548,#3549,#3550,#3551,#3552,#3553)) ;
#849 = EDGE_LOOP('',(#3554)) ;
#850 = EDGE_LOOP('',(#3555,#3556,#3557,#3558)) ;
#851 = EDGE_LOOP('',(#3559,#3560,#3561,#3562)) ;
#852 = EDGE_LOOP('',(#3563,#3564,#3565,#3566)) ;
#853 = EDGE_LOOP('',(#3567)) ;
#854 = EDGE_LOOP('',(#3568,#3569,#3570,#3571)) ;
#855 = EDGE_LOOP('',(#3572,#3573,#3574,#3575,#3576,#3577,#3578,#3579)) ;
#856 = EDGE_LOOP('',(#3580)) ;
#857 = EDGE_LOOP('',(#3581,#3582,#3583,#3584)) ;
#858 = EDGE_LOOP('',(#3585,#3586,#3587,#3588,#3589,#3590,#3591)) ;
#859 = EDGE_LOOP('',(#3592,#3593,#3594,#3595)) ;
#860 = EDGE_LOOP('',(#3596,#3597,#3598,#3599)) ;
#861 = EDGE_LOOP('',(#3600,#3601,#3602,#3603)) ;
#862 = EDGE_LOOP('',(#3604,#3605,#3606,#3607)) ;
#863 = EDGE_LOOP('',(#3608,#3609,#3610,#3611)) ;
#864 = EDGE_LOOP('',(#3612,#3613,#3614,#3615)) ;
#865 = EDGE_LOOP('',(#3616,#3617,#3618,#3619)) ;
#866 = EDGE_LOOP('',(#3620,#3621,#3622,#3623,#3624,#3625)) ;
#867 = EDGE_LOOP('',(#3626)) ;
#868 = EDGE_LOOP('',(#3627,#3628,#3629,#3630)) ;
#869 = EDGE_LOOP('',(#3631,#3632,#3633,#3634,#3635)) ;
#870 = EDGE_LOOP('',(#3636,#3637,#3638,#3639,#3640)) ;
#871 = EDGE_LOOP('',(#3641,#3642,#3643,#3644,#3645)) ;
#872 = EDGE_LOOP('',(#3646,#3647,#3648,#3649,#3650,#3651)) ;
#873 = EDGE_LOOP('',(#3652,#3653,#3654,#3655)) ;
#874 = EDGE_LOOP('',(#3656)) ;
#875 = EDGE_LOOP('',(#3657,#3658,#3659,#3660,#3661)) ;
#876 = EDGE_LOOP('',(#3662,#3663,#3664,#3665)) ;
#877 = EDGE_LOOP('',(#3666,#3667,#3668,#3669)) ;
#878 = EDGE_LOOP('',(#3670,#3671,#3672,#3673)) ;
#879 = EDGE_LOOP('',(#3674,#3675,#3676,#3677)) ;
#880 = EDGE_LOOP('',(#3678,#3679,#3680,#3681)) ;
#881 = EDGE_LOOP('',(#3682,#3683,#3684,#3685)) ;
#882 = EDGE_LOOP('',(#3686,#3687,#3688,#3689)) ;
#883 = EDGE_LOOP('',(#3690,#3691,#3692,#3693)) ;
#884 = EDGE_LOOP('',(#3694,#3695,#3696,#3697)) ;
#885 = EDGE_LOOP('',(#3698,#3699,#3700,#3701)) ;
#886 = EDGE_LOOP('',(#3702,#3703,#3704,#3705)) ;
#887 = EDGE_LOOP('',(#3706,#3707,#3708,#3709)) ;
#888 = EDGE_LOOP('',(#3710,#3711,#3712,#3713)) ;
#889 = EDGE_LOOP('',(#3714,#3715,#3716,#3717,#3718)) ;
#890 = EDGE_LOOP('',(#3719,#3720,#3721,#3722)) ;
#891 = EDGE_LOOP('',(#3723,#3724,#3725,#3726)) ;
#892 = EDGE_LOOP('',(#3727,#3728,#3729,#3730)) ;
#893 = EDGE_LOOP('',(#3731,#3732,#3733,#3734)) ;
#894 = EDGE_LOOP('',(#3735,#3736,#3737,#3738,#3739)) ;
#895 = EDGE_LOOP('',(#3740,#3741,#3742,#3743)) ;
#896 = EDGE_LOOP('',(#3744,#3745,#3746,#3747)) ;
#897 = EDGE_LOOP('',(#3748,#3749,#3750,#3751)) ;
#898 = EDGE_LOOP('',(#3752,#3753,#3754,#3755)) ;
#899 = EDGE_LOOP('',(#3756,#3757,#3758,#3759)) ;
#900 = EDGE_LOOP('',(#3760,#3761,#3762,#3763)) ;
#901 = EDGE_LOOP('',(#3764,#3765,#3766,#3767)) ;
#902 = EDGE_LOOP('',(#3768,#3769,#3770,#3771)) ;
#903 = EDGE_LOOP('',(#3772,#3773,#3774)) ;
#904 = EDGE_LOOP('',(#3775,#3776,#3777)) ;
#905 = EDGE_LOOP('',(#3778,#3779,#3780,#3781,#3782,#3783,#3784)) ;
#906 = EDGE_LOOP('',(#3785)) ;
#907 = EDGE_LOOP('',(#3786,#3787,#3788,#3789,#3790)) ;
#908 = EDGE_LOOP('',(#3791,#3792)) ;
#909 = EDGE_LOOP('',(#3793,#3794,#3795,#3796,#3797,#3798,#3799,#3800)) ;
#910 = EDGE_LOOP('',(#3801,#3802,#3803,#3804,#3805)) ;
#911 = EDGE_LOOP('',(#3806,#3807,#3808,#3809,#3810,#3811,#3812)) ;
#912 = EDGE_LOOP('',(#3813)) ;
#913 = EDGE_LOOP('',(#3814,#3815,#3816,#3817,#3818,#3819,#3820)) ;
#914 = EDGE_LOOP('',(#3821,#3822,#3823,#3824)) ;
#915 = EDGE_LOOP('',(#3825,#3826,#3827,#3828)) ;
#916 = EDGE_LOOP('',(#3829,#3830,#3831,#3832,#3833)) ;
#917 = EDGE_LOOP('',(#3834,#3835,#3836,#3837)) ;
#918 = EDGE_LOOP('',(#3838,#3839,#3840,#3841)) ;
#919 = EDGE_LOOP('',(#3842,#3843,#3844,#3845)) ;
#920 = EDGE_LOOP('',(#3846,#3847,#3848,#3849)) ;
#921 = EDGE_LOOP('',(#3850,#3851,#3852,#3853)) ;
#922 = EDGE_LOOP('',(#3854,#3855,#3856,#3857,#3858)) ;
#923 = EDGE_LOOP('',(#3859,#3860,#3861,#3862)) ;
#924 = EDGE_LOOP('',(#3863,#3864,#3865,#3866)) ;
#925 = EDGE_LOOP('',(#3867,#3868,#3869,#3870,#3871,#3872)) ;
#926 = EDGE_LOOP('',(#3873)) ;
#927 = EDGE_LOOP('',(#3874,#3875,#3876,#3877)) ;
#928 = EDGE_LOOP('',(#3878,#3879,#3880,#3881)) ;
#929 = EDGE_LOOP('',(#3882,#3883,#3884,#3885)) ;
#930 = EDGE_LOOP('',(#3886,#3887,#3888,#3889)) ;
#931 = EDGE_LOOP('',(#3890,#3891,#3892,#3893)) ;
#932 = EDGE_LOOP('',(#3894,#3895,#3896,#3897)) ;
#933 = EDGE_LOOP('',(#3898,#3899,#3900,#3901)) ;
#934 = EDGE_LOOP('',(#3902,#3903,#3904,#3905,#3906,#3907,#3908,#3909,#3910,
#3911)) ;
#935 = EDGE_LOOP('',(#3912,#3913,#3914,#3915)) ;
#936 = EDGE_LOOP('',(#3916,#3917,#3918,#3919)) ;
#937 = EDGE_LOOP('',(#3920,#3921,#3922,#3923)) ;
#938 = EDGE_LOOP('',(#3924,#3925,#3926,#3927)) ;
#939 = EDGE_LOOP('',(#3928,#3929,#3930,#3931,#3932,#3933,#3934,#3935,#3936,
#3937,#3938,#3939,#3940,#3941,#3942,#3943)) ;
#940 = EDGE_LOOP('',(#3944,#3945,#3946,#3947)) ;
#941 = EDGE_LOOP('',(#3948,#3949,#3950,#3951,#3952,#3953,#3954,#3955,#3956,
#3957)) ;
#942 = EDGE_LOOP('',(#3958)) ;
#943 = EDGE_LOOP('',(#3959,#3960,#3961,#3962)) ;
#944 = EDGE_LOOP('',(#3963)) ;
#945 = EDGE_LOOP('',(#3964,#3965,#3966,#3967)) ;
#946 = EDGE_LOOP('',(#3968,#3969,#3970,#3971,#3972)) ;
#947 = EDGE_LOOP('',(#3973,#3974,#3975,#3976)) ;
#948 = EDGE_LOOP('',(#3977,#3978,#3979,#3980,#3981,#3982)) ;
#949 = EDGE_LOOP('',(#3983)) ;
#950 = EDGE_LOOP('',(#3984,#3985,#3986,#3987)) ;
#951 = EDGE_LOOP('',(#3988,#3989,#3990,#3991,#3992)) ;
#952 = EDGE_LOOP('',(#3993,#3994,#3995,#3996,#3997,#3998)) ;
#953 = EDGE_LOOP('',(#3999)) ;
#954 = EDGE_LOOP('',(#4000,#4001,#4002,#4003)) ;
#955 = EDGE_LOOP('',(#4004,#4005,#4006,#4007)) ;
#956 = EDGE_LOOP('',(#4008,#4009,#4010,#4011)) ;
#957 = EDGE_LOOP('',(#4012,#4013,#4014,#4015)) ;
#958 = EDGE_LOOP('',(#4016,#4017,#4018,#4019)) ;
#959 = EDGE_LOOP('',(#4020,#4021,#4022,#4023)) ;
#960 = EDGE_LOOP('',(#4024,#4025,#4026,#4027,#4028,#4029,#4030,#4031,#4032,
#4033,#4034,#4035)) ;
#961 = EDGE_LOOP('',(#4036,#4037,#4038,#4039)) ;
#962 = EDGE_LOOP('',(#4040,#4041,#4042,#4043)) ;
#963 = EDGE_LOOP('',(#4044,#4045,#4046,#4047)) ;
#964 = EDGE_LOOP('',(#4048,#4049,#4050,#4051)) ;
#965 = EDGE_LOOP('',(#4052,#4053,#4054,#4055)) ;
#966 = EDGE_LOOP('',(#4056,#4057,#4058,#4059)) ;
#967 = EDGE_LOOP('',(#4060,#4061,#4062,#4063)) ;
#968 = EDGE_LOOP('',(#4064,#4065,#4066,#4067)) ;
#969 = EDGE_LOOP('',(#4068,#4069,#4070,#4071)) ;
#970 = EDGE_LOOP('',(#4072,#4073,#4074,#4075,#4076,#4077)) ;
#971 = EDGE_LOOP('',(#4078,#4079,#4080,#4081)) ;
#972 = EDGE_LOOP('',(#4082,#4083,#4084,#4085)) ;
#973 = EDGE_LOOP('',(#4086,#4087,#4088,#4089)) ;
#974 = EDGE_LOOP('',(#4090,#4091,#4092,#4093)) ;
#975 = EDGE_LOOP('',(#4094,#4095,#4096,#4097)) ;
#976 = EDGE_LOOP('',(#4098,#4099,#4100,#4101)) ;
#977 = EDGE_LOOP('',(#4102,#4103,#4104,#4105)) ;
#978 = EDGE_LOOP('',(#4106,#4107,#4108,#4109)) ;
#979 = EDGE_LOOP('',(#4110,#4111,#4112,#4113)) ;
#980 = EDGE_LOOP('',(#4114,#4115,#4116,#4117,#4118,#4119,#4120)) ;
#981 = EDGE_LOOP('',(#4121,#4122,#4123,#4124)) ;
#982 = EDGE_LOOP('',(#4125,#4126,#4127,#4128)) ;
#983 = EDGE_LOOP('',(#4129,#4130,#4131,#4132)) ;
#984 = EDGE_LOOP('',(#4133,#4134,#4135,#4136)) ;
#985 = EDGE_LOOP('',(#4137,#4138,#4139,#4140)) ;
#986 = EDGE_LOOP('',(#4141,#4142,#4143,#4144)) ;
#987 = EDGE_LOOP('',(#4145,#4146,#4147,#4148)) ;
#988 = EDGE_LOOP('',(#4149,#4150,#4151,#4152,#4153,#4154,#4155)) ;
#989 = EDGE_LOOP('',(#4156,#4157,#4158,#4159)) ;
#990 = EDGE_LOOP('',(#4160,#4161,#4162,#4163)) ;
#991 = EDGE_LOOP('',(#4164,#4165,#4166,#4167,#4168,#4169,#4170)) ;
#992 = EDGE_LOOP('',(#4171)) ;
#993 = EDGE_LOOP('',(#4172,#4173,#4174,#4175)) ;
#994 = EDGE_LOOP('',(#4176,#4177,#4178,#4179)) ;
#995 = EDGE_LOOP('',(#4180,#4181,#4182,#4183)) ;
#996 = EDGE_LOOP('',(#4184,#4185,#4186,#4187)) ;
#997 = EDGE_LOOP('',(#4188,#4189,#4190,#4191,#4192,#4193,#4194)) ;
#998 = EDGE_LOOP('',(#4195)) ;
#999 = EDGE_LOOP('',(#4196,#4197,#4198,#4199,#4200,#4201,#4202,#4203,#4204,
#4205,#4206,#4207)) ;
#1000 = EDGE_LOOP('',(#4208,#4209,#4210,#4211)) ;
#1001 = EDGE_LOOP('',(#4212,#4213,#4214,#4215)) ;
#1002 = EDGE_LOOP('',(#4216,#4217,#4218,#4219)) ;
#1003 = EDGE_LOOP('',(#4220,#4221,#4222,#4223,#4224,#4225,#4226,#4227)) ;
#1004 = EDGE_LOOP('',(#4228,#4229,#4230,#4231)) ;
#1005 = EDGE_LOOP('',(#4232,#4233,#4234,#4235)) ;
#1006 = EDGE_LOOP('',(#4236,#4237,#4238,#4239)) ;
#1007 = EDGE_LOOP('',(#4240,#4241,#4242,#4243)) ;
#1008 = EDGE_LOOP('',(#4244,#4245,#4246,#4247)) ;
#1009 = EDGE_LOOP('',(#4248,#4249,#4250,#4251)) ;
#1010 = EDGE_LOOP('',(#4252,#4253,#4254,#4255)) ;
#1011 = EDGE_LOOP('',(#4256,#4257,#4258,#4259)) ;
#1012 = EDGE_LOOP('',(#4260,#4261,#4262,#4263)) ;
#1013 = EDGE_LOOP('',(#4264,#4265,#4266,#4267)) ;
#1014 = EDGE_LOOP('',(#4268,#4269,#4270,#4271)) ;
#1015 = EDGE_LOOP('',(#4272,#4273,#4274,#4275)) ;
#1016 = EDGE_LOOP('',(#4276,#4277,#4278,#4279)) ;
#1017 = EDGE_LOOP('',(#4280,#4281,#4282,#4283)) ;
#1018 = EDGE_LOOP('',(#4284,#4285,#4286,#4287)) ;
#1019 = EDGE_LOOP('',(#4288,#4289,#4290,#4291)) ;
#1020 = EDGE_LOOP('',(#4292,#4293,#4294,#4295)) ;
#1021 = EDGE_LOOP('',(#4296,#4297,#4298,#4299)) ;
#1022 = EDGE_LOOP('',(#4300,#4301,#4302,#4303)) ;
#1023 = EDGE_LOOP('',(#4304,#4305,#4306,#4307)) ;
#1024 = EDGE_LOOP('',(#4308,#4309,#4310,#4311)) ;
#1025 = EDGE_LOOP('',(#4312,#4313,#4314,#4315)) ;
#1026 = EDGE_LOOP('',(#4316,#4317,#4318,#4319)) ;
#1027 = EDGE_LOOP('',(#4320,#4321,#4322,#4323)) ;
#1028 = EDGE_LOOP('',(#4324,#4325,#4326,#4327)) ;
#1029 = EDGE_LOOP('',(#4328,#4329,#4330,#4331)) ;
#1030 = EDGE_LOOP('',(#4332,#4333,#4334,#4335)) ;
#1031 = EDGE_LOOP('',(#4336,#4337,#4338,#4339)) ;
#1032 = EDGE_LOOP('',(#4340,#4341,#4342,#4343)) ;
#1033 = EDGE_LOOP('',(#4344,#4345,#4346,#4347)) ;
#1034 = EDGE_LOOP('',(#4348,#4349,#4350,#4351)) ;
#1035 = EDGE_LOOP('',(#4352,#4353,#4354,#4355)) ;
#1036 = EDGE_LOOP('',(#4356,#4357,#4358,#4359)) ;
#1037 = EDGE_LOOP('',(#4360,#4361,#4362,#4363)) ;
#1038 = EDGE_LOOP('',(#4364,#4365,#4366,#4367)) ;
#1039 = EDGE_LOOP('',(#4368,#4369,#4370,#4371)) ;
#1040 = EDGE_LOOP('',(#4372,#4373,#4374,#4375)) ;
#1041 = EDGE_LOOP('',(#4376,#4377,#4378,#4379)) ;
#1042 = EDGE_LOOP('',(#4380,#4381,#4382,#4383)) ;
#1043 = EDGE_LOOP('',(#4384,#4385,#4386,#4387)) ;
#1044 = EDGE_LOOP('',(#4388,#4389,#4390,#4391)) ;
#1045 = EDGE_LOOP('',(#4392,#4393,#4394,#4395)) ;
#1046 = EDGE_LOOP('',(#4396,#4397,#4398,#4399)) ;
#1047 = EDGE_LOOP('',(#4400,#4401,#4402,#4403)) ;
#1048 = EDGE_LOOP('',(#4404,#4405,#4406,#4407)) ;
#1049 = EDGE_LOOP('',(#4408,#4409,#4410,#4411)) ;
#1050 = EDGE_LOOP('',(#4412,#4413,#4414,#4415)) ;
#1051 = EDGE_LOOP('',(#4416,#4417,#4418,#4419)) ;
#1052 = EDGE_LOOP('',(#4420,#4421,#4422,#4423,#4424,#4425,#4426,#4427,#4428,
#4429,#4430,#4431,#4432,#4433,#4434,#4435,#4436,#4437,#4438,#4439,#4440,
#4441,#4442,#4443,#4444,#4445,#4446,#4447,#4448)) ;
#1053 = EDGE_LOOP('',(#4449,#4450,#4451,#4452)) ;
#1054 = EDGE_LOOP('',(#4453)) ;
#1055 = EDGE_LOOP('',(#4454,#4455,#4456,#4457)) ;
#1056 = EDGE_LOOP('',(#4458,#4459,#4460,#4461)) ;
#1057 = EDGE_LOOP('',(#4462,#4463,#4464,#4465)) ;
#1058 = EDGE_LOOP('',(#4466,#4467,#4468,#4469)) ;
#1059 = EDGE_LOOP('',(#4470,#4471,#4472,#4473)) ;
#1060 = EDGE_LOOP('',(#4474,#4475,#4476,#4477)) ;
#1061 = EDGE_LOOP('',(#4478,#4479,#4480,#4481)) ;
#1062 = EDGE_LOOP('',(#4482,#4483,#4484,#4485)) ;
#1063 = EDGE_LOOP('',(#4486,#4487,#4488,#4489)) ;
#1064 = EDGE_LOOP('',(#4490,#4491,#4492,#4493)) ;
#1065 = EDGE_LOOP('',(#4494,#4495,#4496,#4497)) ;
#1066 = EDGE_LOOP('',(#4498,#4499,#4500,#4501)) ;
#1067 = EDGE_LOOP('',(#4502,#4503,#4504,#4505)) ;
#1068 = EDGE_LOOP('',(#4506,#4507,#4508,#4509)) ;
#1069 = EDGE_LOOP('',(#4510,#4511,#4512,#4513)) ;
#1070 = EDGE_LOOP('',(#4514,#4515,#4516,#4517)) ;
#1071 = EDGE_LOOP('',(#4518,#4519,#4520,#4521)) ;
#1072 = EDGE_LOOP('',(#4522,#4523,#4524,#4525)) ;
#1073 = EDGE_LOOP('',(#4526,#4527,#4528,#4529)) ;
#1074 = EDGE_LOOP('',(#4530,#4531,#4532,#4533)) ;
#1075 = EDGE_LOOP('',(#4534,#4535,#4536,#4537)) ;
#1076 = EDGE_LOOP('',(#4538,#4539,#4540,#4541)) ;
#1077 = EDGE_LOOP('',(#4542,#4543,#4544,#4545)) ;
#1078 = EDGE_LOOP('',(#4546,#4547,#4548,#4549)) ;
#1079 = EDGE_LOOP('',(#4550,#4551,#4552,#4553)) ;
#1080 = EDGE_LOOP('',(#4554,#4555,#4556,#4557)) ;
#1081 = EDGE_LOOP('',(#4558,#4559,#4560,#4561)) ;
#1082 = EDGE_LOOP('',(#4562,#4563,#4564,#4565)) ;
#1083 = EDGE_LOOP('',(#4566,#4567,#4568,#4569)) ;
#1084 = EDGE_LOOP('',(#4570,#4571,#4572,#4573)) ;
#1085 = EDGE_LOOP('',(#4574,#4575,#4576,#4577)) ;
#1086 = EDGE_LOOP('',(#4578,#4579,#4580,#4581)) ;
#1087 = EDGE_LOOP('',(#4582,#4583,#4584,#4585)) ;
#1088 = EDGE_LOOP('',(#4586,#4587,#4588,#4589)) ;
#1089 = EDGE_LOOP('',(#4590,#4591,#4592,#4593)) ;
#1090 = EDGE_LOOP('',(#4594,#4595,#4596,#4597)) ;
#1091 = EDGE_LOOP('',(#4598,#4599,#4600,#4601)) ;
#1092 = EDGE_LOOP('',(#4602,#4603,#4604,#4605)) ;
#1093 = EDGE_LOOP('',(#4606,#4607,#4608,#4609)) ;
#1094 = EDGE_LOOP('',(#4610,#4611,#4612,#4613)) ;
#1095 = EDGE_LOOP('',(#4614,#4615,#4616,#4617)) ;
#1096 = EDGE_LOOP('',(#4618,#4619,#4620,#4621)) ;
#1097 = EDGE_LOOP('',(#4622,#4623,#4624,#4625)) ;
#1098 = EDGE_LOOP('',(#4626,#4627,#4628,#4629,#4630,#4631,#4632,#4633,#4634,
#4635,#4636,#4637,#4638,#4639,#4640,#4641,#4642,#4643,#4644,#4645,#4646,
#4647,#4648,#4649,#4650,#4651,#4652,#4653,#4654)) ;
#1099 = EDGE_LOOP('',(#4655,#4656,#4657,#4658)) ;
#1100 = EDGE_LOOP('',(#4659)) ;
#1101 = EDGE_LOOP('',(#4660,#4661,#4662,#4663)) ;
#1102 = EDGE_LOOP('',(#4664,#4665,#4666,#4667)) ;
#1103 = EDGE_LOOP('',(#4668,#4669,#4670,#4671)) ;
#1104 = EDGE_LOOP('',(#4672,#4673,#4674,#4675)) ;
#1105 = EDGE_LOOP('',(#4676,#4677,#4678,#4679)) ;
#1106 = EDGE_LOOP('',(#4680,#4681,#4682,#4683)) ;
#1107 = EDGE_LOOP('',(#4684,#4685,#4686,#4687)) ;
#1108 = EDGE_LOOP('',(#4688,#4689,#4690,#4691)) ;
#1109 = EDGE_LOOP('',(#4692,#4693,#4694,#4695)) ;
#1110 = EDGE_LOOP('',(#4696,#4697,#4698,#4699)) ;
#1111 = EDGE_LOOP('',(#4700,#4701,#4702,#4703)) ;
#1112 = EDGE_LOOP('',(#4704,#4705,#4706,#4707)) ;
#1113 = EDGE_LOOP('',(#4708,#4709,#4710,#4711)) ;
#1114 = EDGE_LOOP('',(#4712)) ;
#1115 = EDGE_LOOP('',(#4713,#4714,#4715,#4716)) ;
#1116 = EDGE_LOOP('',(#4717,#4718,#4719,#4720)) ;
#1117 = EDGE_LOOP('',(#4721,#4722,#4723,#4724)) ;
#1118 = EDGE_LOOP('',(#4725)) ;
#1119 = EDGE_LOOP('',(#4726)) ;
#1120 = EDGE_LOOP('',(#4727,#4728,#4729,#4730)) ;
#1121 = EDGE_LOOP('',(#4731)) ;
#1122 = EDGE_LOOP('',(#4732)) ;
#1123 = EDGE_LOOP('',(#4733,#4734,#4735,#4736)) ;
#1124 = EDGE_LOOP('',(#4737,#4738,#4739,#4740)) ;
#1125 = EDGE_LOOP('',(#4741,#4742,#4743,#4744)) ;
#1126 = EDGE_LOOP('',(#4745)) ;
#1127 = EDGE_LOOP('',(#4746)) ;
#1128 = EDGE_LOOP('',(#4747,#4748,#4749,#4750)) ;
#1129 = EDGE_LOOP('',(#4751)) ;
#1130 = EDGE_LOOP('',(#4752)) ;
#1131 = EDGE_LOOP('',(#4753,#4754,#4755,#4756)) ;
#1132 = EDGE_LOOP('',(#4757,#4758,#4759,#4760)) ;
#1133 = EDGE_LOOP('',(#4761,#4762,#4763,#4764)) ;
#1134 = EDGE_LOOP('',(#4765)) ;
#1135 = EDGE_LOOP('',(#4766,#4767,#4768,#4769)) ;
#1136 = EDGE_LOOP('',(#4770,#4771,#4772,#4773)) ;
#1137 = EDGE_LOOP('',(#4774,#4775,#4776,#4777)) ;
#1138 = EDGE_LOOP('',(#4778,#4779,#4780,#4781)) ;
#1139 = EDGE_LOOP('',(#4782,#4783,#4784,#4785)) ;
#1140 = EDGE_LOOP('',(#4786,#4787,#4788,#4789)) ;
#1141 = EDGE_LOOP('',(#4790,#4791,#4792,#4793)) ;
#1142 = EDGE_LOOP('',(#4794,#4795,#4796,#4797)) ;
#1143 = EDGE_LOOP('',(#4798,#4799,#4800,#4801)) ;
#1144 = EDGE_LOOP('',(#4802,#4803,#4804,#4805)) ;
#1145 = EDGE_LOOP('',(#4806,#4807,#4808,#4809,#4810,#4811,#4812,#4813,#4814)) ;
#1146 = EDGE_LOOP('',(#4815)) ;
#1147 = EDGE_LOOP('',(#4816,#4817,#4818,#4819,#4820,#4821,#4822,#4823,#4824)) ;
#1148 = EDGE_LOOP('',(#4825)) ;
#1149 = EDGE_LOOP('',(#4826,#4827,#4828,#4829)) ;
#1150 = EDGE_LOOP('',(#4830,#4831,#4832,#4833)) ;
#1151 = EDGE_LOOP('',(#4834,#4835,#4836,#4837)) ;
#1152 = EDGE_LOOP('',(#4838,#4839,#4840,#4841)) ;
#1153 = EDGE_LOOP('',(#4842,#4843,#4844,#4845)) ;
#1154 = EDGE_LOOP('',(#4846,#4847,#4848,#4849)) ;
#1155 = EDGE_LOOP('',(#4850,#4851,#4852,#4853,#4854,#4855)) ;
#1156 = EDGE_LOOP('',(#4856)) ;
#1157 = EDGE_LOOP('',(#4857,#4858,#4859,#4860,#4861,#4862)) ;
#1158 = EDGE_LOOP('',(#4863,#4864,#4865,#4866)) ;
#1159 = EDGE_LOOP('',(#4867,#4868,#4869,#4870)) ;
#1160 = EDGE_LOOP('',(#4871,#4872,#4873,#4874)) ;
#1161 = EDGE_LOOP('',(#4875,#4876,#4877,#4878)) ;
#1162 = EDGE_LOOP('',(#4879,#4880,#4881,#4882)) ;
#1163 = EDGE_LOOP('',(#4883)) ;
#1164 = EDGE_LOOP('',(#4884,#4885,#4886,#4887,#4888,#4889,#4890)) ;
#1165 = EDGE_LOOP('',(#4891,#4892,#4893)) ;
#1166 = EDGE_LOOP('',(#4894,#4895,#4896,#4897,#4898,#4899,#4900)) ;
#1167 = EDGE_LOOP('',(#4901,#4902,#4903,#4904,#4905,#4906,#4907,#4908,#4909)) ;
#1168 = EDGE_LOOP('',(#4910,#4911,#4912,#4913,#4914,#4915)) ;
#1169 = EDGE_LOOP('',(#4916,#4917,#4918)) ;
#1170 = EDGE_LOOP('',(#4919,#4920,#4921,#4922)) ;
#1171 = EDGE_LOOP('',(#4923,#4924,#4925,#4926,#4927,#4928,#4929)) ;
#1172 = EDGE_LOOP('',(#4930,#4931,#4932,#4933)) ;
#1173 = EDGE_LOOP('',(#4934)) ;
#1174 = EDGE_LOOP('',(#4935)) ;
#1175 = EDGE_LOOP('',(#4936,#4937,#4938,#4939)) ;
#1176 = EDGE_LOOP('',(#4940)) ;
#1177 = EDGE_LOOP('',(#4941)) ;
#1178 = EDGE_LOOP('',(#4942,#4943,#4944,#4945)) ;
#1179 = EDGE_LOOP('',(#4946)) ;
#1180 = EDGE_LOOP('',(#4947)) ;
#1181 = EDGE_LOOP('',(#4948,#4949,#4950,#4951)) ;
#1182 = EDGE_LOOP('',(#4952)) ;
#1183 = EDGE_LOOP('',(#4953)) ;
#1184 = EDGE_LOOP('',(#4954,#4955,#4956,#4957)) ;
#1185 = EDGE_LOOP('',(#4958)) ;
#1186 = EDGE_LOOP('',(#4959)) ;
#1187 = EDGE_LOOP('',(#4960,#4961,#4962,#4963)) ;
#1188 = EDGE_LOOP('',(#4964)) ;
#1189 = EDGE_LOOP('',(#4965)) ;
#1190 = EDGE_LOOP('',(#4966,#4967,#4968,#4969)) ;
#1191 = EDGE_LOOP('',(#4970,#4971,#4972,#4973)) ;
#1192 = EDGE_LOOP('',(#4974,#4975,#4976,#4977)) ;
#1193 = EDGE_LOOP('',(#4978,#4979,#4980,#4981)) ;
#1194 = EDGE_LOOP('',(#4982,#4983,#4984,#4985)) ;
#1195 = EDGE_LOOP('',(#4986,#4987,#4988,#4989)) ;
#1196 = EDGE_LOOP('',(#4990,#4991,#4992,#4993)) ;
#1197 = EDGE_LOOP('',(#4994,#4995,#4996,#4997)) ;
#1198 = EDGE_LOOP('',(#4998,#4999,#5000,#5001,#5002,#5003,#5004,#5005)) ;
#1199 = EDGE_LOOP('',(#5006,#5007,#5008,#5009,#5010,#5011,#5012,#5013)) ;
#1200 = EDGE_LOOP('',(#5014,#5015,#5016,#5017)) ;
#1201 = EDGE_LOOP('',(#5018,#5019,#5020,#5021)) ;
#1202 = EDGE_LOOP('',(#5022,#5023,#5024,#5025)) ;
#1203 = EDGE_LOOP('',(#5026,#5027,#5028,#5029)) ;
#1204 = EDGE_LOOP('',(#5030,#5031,#5032,#5033)) ;
#1205 = EDGE_LOOP('',(#5034,#5035,#5036,#5037)) ;
#1206 = EDGE_LOOP('',(#5038,#5039,#5040,#5041)) ;
#1207 = EDGE_LOOP('',(#5042,#5043,#5044,#5045)) ;
#1208 = EDGE_LOOP('',(#5046,#5047,#5048,#5049)) ;
#1209 = EDGE_LOOP('',(#5050,#5051,#5052,#5053)) ;
#1210 = EDGE_LOOP('',(#5054,#5055,#5056,#5057)) ;
#1211 = EDGE_LOOP('',(#5058,#5059,#5060,#5061,#5062,#5063,#5064,#5065,#5066,
#5067)) ;
#1212 = EDGE_LOOP('',(#5068)) ;
#1213 = EDGE_LOOP('',(#5069,#5070,#5071,#5072,#5073,#5074,#5075,#5076,#5077,
#5078)) ;
#1214 = EDGE_LOOP('',(#5079)) ;
#1215 = EDGE_LOOP('',(#5080,#5081,#5082,#5083)) ;
#1216 = EDGE_LOOP('',(#5084)) ;
#1217 = EDGE_LOOP('',(#5085)) ;
#1218 = EDGE_LOOP('',(#5086,#5087,#5088,#5089)) ;
#1219 = EDGE_LOOP('',(#5090)) ;
#1220 = EDGE_LOOP('',(#5091)) ;
#1221 = LINE('',#8134,#1604) ;
#1222 = LINE('',#8140,#1605) ;
#1223 = LINE('',#8146,#1606) ;
#1224 = LINE('',#8153,#1607) ;
#1225 = LINE('',#8155,#1608) ;
#1226 = LINE('',#8157,#1609) ;
#1227 = LINE('',#8160,#1610) ;
#1228 = LINE('',#8163,#1611) ;
#1229 = LINE('',#8165,#1612) ;
#1230 = LINE('',#8167,#1613) ;
#1231 = LINE('',#8169,#1614) ;
#1232 = LINE('',#8171,#1615) ;
#1233 = LINE('',#8173,#1616) ;
#1234 = LINE('',#8174,#1617) ;
#1235 = LINE('',#8177,#1618) ;
#1236 = LINE('',#8178,#1619) ;
#1237 = LINE('',#8181,#1620) ;
#1238 = LINE('',#8182,#1621) ;
#1239 = LINE('',#8185,#1622) ;
#1240 = LINE('',#8186,#1623) ;
#1241 = LINE('',#8189,#1624) ;
#1242 = LINE('',#8190,#1625) ;
#1243 = LINE('',#8193,#1626) ;
#1244 = LINE('',#8195,#1627) ;
#1245 = LINE('',#8196,#1628) ;
#1246 = LINE('',#8199,#1629) ;
#1247 = LINE('',#8201,#1630) ;
#1248 = LINE('',#8202,#1631) ;
#1249 = LINE('',#8209,#1632) ;
#1250 = LINE('',#8213,#1633) ;
#1251 = LINE('',#8247,#1634) ;
#1252 = LINE('',#8248,#1635) ;
#1253 = LINE('',#8256,#1636) ;
#1254 = LINE('',#8257,#1637) ;
#1255 = LINE('',#8260,#1638) ;
#1256 = LINE('',#8262,#1639) ;
#1257 = LINE('',#8263,#1640) ;
#1258 = LINE('',#8266,#1641) ;
#1259 = LINE('',#8273,#1642) ;
#1260 = LINE('',#8277,#1643) ;
#1261 = LINE('',#8279,#1644) ;
#1262 = LINE('',#8280,#1645) ;
#1263 = LINE('',#8291,#1646) ;
#1264 = LINE('',#8304,#1647) ;
#1265 = LINE('',#8306,#1648) ;
#1266 = LINE('',#8310,#1649) ;
#1267 = LINE('',#8313,#1650) ;
#1268 = LINE('',#8318,#1651) ;
#1269 = LINE('',#8321,#1652) ;
#1270 = LINE('',#8324,#1653) ;
#1271 = LINE('',#8335,#1654) ;
#1272 = LINE('',#8341,#1655) ;
#1273 = LINE('',#8344,#1656) ;
#1274 = LINE('',#8346,#1657) ;
#1275 = LINE('',#8347,#1658) ;
#1276 = LINE('',#8350,#1659) ;
#1277 = LINE('',#8384,#1660) ;
#1278 = LINE('',#8385,#1661) ;
#1279 = LINE('',#8390,#1662) ;
#1280 = LINE('',#8497,#1663) ;
#1281 = LINE('',#8717,#1664) ;
#1282 = LINE('',#8720,#1665) ;
#1283 = LINE('',#8725,#1666) ;
#1284 = LINE('',#8730,#1667) ;
#1285 = LINE('',#8742,#1668) ;
#1286 = LINE('',#8743,#1669) ;
#1287 = LINE('',#8799,#1670) ;
#1288 = LINE('',#8801,#1671) ;
#1289 = LINE('',#8803,#1672) ;
#1290 = LINE('',#8806,#1673) ;
#1291 = LINE('',#8810,#1674) ;
#1292 = LINE('',#8814,#1675) ;
#1293 = LINE('',#8816,#1676) ;
#1294 = LINE('',#8819,#1677) ;
#1295 = LINE('',#8821,#1678) ;
#1296 = LINE('',#8825,#1679) ;
#1297 = LINE('',#8826,#1680) ;
#1298 = LINE('',#8902,#1681) ;
#1299 = LINE('',#8929,#1682) ;
#1300 = LINE('',#8931,#1683) ;
#1301 = LINE('',#8934,#1684) ;
#1302 = LINE('',#8935,#1685) ;
#1303 = LINE('',#8938,#1686) ;
#1304 = LINE('',#8942,#1687) ;
#1305 = LINE('',#8943,#1688) ;
#1306 = LINE('',#8946,#1689) ;
#1307 = LINE('',#9043,#1690) ;
#1308 = LINE('',#9044,#1691) ;
#1309 = LINE('',#9049,#1692) ;
#1310 = LINE('',#9050,#1693) ;
#1311 = LINE('',#9055,#1694) ;
#1312 = LINE('',#9057,#1695) ;
#1313 = LINE('',#9058,#1696) ;
#1314 = LINE('',#9061,#1697) ;
#1315 = LINE('',#9065,#1698) ;
#1316 = LINE('',#9066,#1699) ;
#1317 = LINE('',#9069,#1700) ;
#1318 = LINE('',#9073,#1701) ;
#1319 = LINE('',#9074,#1702) ;
#1320 = LINE('',#9077,#1703) ;
#1321 = LINE('',#9081,#1704) ;
#1322 = LINE('',#9082,#1705) ;
#1323 = LINE('',#9085,#1706) ;
#1324 = LINE('',#9089,#1707) ;
#1325 = LINE('',#9090,#1708) ;
#1326 = LINE('',#9109,#1709) ;
#1327 = LINE('',#9113,#1710) ;
#1328 = LINE('',#9130,#1711) ;
#1329 = LINE('',#9133,#1712) ;
#1330 = LINE('',#9154,#1713) ;
#1331 = LINE('',#9156,#1714) ;
#1332 = LINE('',#9169,#1715) ;
#1333 = LINE('',#9173,#1716) ;
#1334 = LINE('',#9190,#1717) ;
#1335 = LINE('',#9191,#1718) ;
#1336 = LINE('',#9199,#1719) ;
#1337 = LINE('',#9200,#1720) ;
#1338 = LINE('',#9203,#1721) ;
#1339 = LINE('',#9205,#1722) ;
#1340 = LINE('',#9206,#1723) ;
#1341 = LINE('',#9209,#1724) ;
#1342 = LINE('',#9213,#1725) ;
#1343 = LINE('',#9217,#1726) ;
#1344 = LINE('',#9225,#1727) ;
#1345 = LINE('',#9228,#1728) ;
#1346 = LINE('',#9229,#1729) ;
#1347 = LINE('',#9234,#1730) ;
#1348 = LINE('',#9237,#1731) ;
#1349 = LINE('',#9247,#1732) ;
#1350 = LINE('',#9253,#1733) ;
#1351 = LINE('',#9256,#1734) ;
#1352 = LINE('',#9258,#1735) ;
#1353 = LINE('',#9259,#1736) ;
#1354 = LINE('',#9262,#1737) ;
#1355 = LINE('',#9265,#1738) ;
#1356 = LINE('',#9267,#1739) ;
#1357 = LINE('',#9314,#1740) ;
#1358 = LINE('',#9321,#1741) ;
#1359 = LINE('',#9343,#1742) ;
#1360 = LINE('',#9350,#1743) ;
#1361 = LINE('',#9353,#1744) ;
#1362 = LINE('',#9355,#1745) ;
#1363 = LINE('',#9357,#1746) ;
#1364 = LINE('',#9358,#1747) ;
#1365 = LINE('',#9361,#1748) ;
#1366 = LINE('',#9365,#1749) ;
#1367 = LINE('',#9366,#1750) ;
#1368 = LINE('',#9369,#1751) ;
#1369 = LINE('',#9373,#1752) ;
#1370 = LINE('',#9377,#1753) ;
#1371 = LINE('',#9381,#1754) ;
#1372 = LINE('',#9382,#1755) ;
#1373 = LINE('',#9385,#1756) ;
#1374 = LINE('',#9389,#1757) ;
#1375 = LINE('',#9391,#1758) ;
#1376 = LINE('',#9392,#1759) ;
#1377 = LINE('',#9395,#1760) ;
#1378 = LINE('',#9400,#1761) ;
#1379 = LINE('',#9403,#1762) ;
#1380 = LINE('',#9405,#1763) ;
#1381 = LINE('',#9407,#1764) ;
#1382 = LINE('',#9411,#1765) ;
#1383 = LINE('',#9416,#1766) ;
#1384 = LINE('',#9417,#1767) ;
#1385 = LINE('',#9418,#1768) ;
#1386 = LINE('',#9421,#1769) ;
#1387 = LINE('',#9422,#1770) ;
#1388 = LINE('',#9426,#1771) ;
#1389 = LINE('',#9429,#1772) ;
#1390 = LINE('',#9430,#1773) ;
#1391 = LINE('',#9433,#1774) ;
#1392 = LINE('',#9436,#1775) ;
#1393 = LINE('',#9439,#1776) ;
#1394 = LINE('',#9442,#1777) ;
#1395 = LINE('',#9445,#1778) ;
#1396 = LINE('',#9448,#1779) ;
#1397 = LINE('',#9454,#1780) ;
#1398 = LINE('',#9469,#1781) ;
#1399 = LINE('',#9509,#1782) ;
#1400 = LINE('',#9523,#1783) ;
#1401 = LINE('',#9543,#1784) ;
#1402 = LINE('',#9557,#1785) ;
#1403 = LINE('',#9604,#1786) ;
#1404 = LINE('',#9606,#1787) ;
#1405 = LINE('',#9638,#1788) ;
#1406 = LINE('',#9665,#1789) ;
#1407 = LINE('',#9712,#1790) ;
#1408 = LINE('',#9730,#1791) ;
#1409 = LINE('',#9734,#1792) ;
#1410 = LINE('',#9762,#1793) ;
#1411 = LINE('',#9862,#1794) ;
#1412 = LINE('',#9863,#1795) ;
#1413 = LINE('',#9865,#1796) ;
#1414 = LINE('',#9866,#1797) ;
#1415 = LINE('',#9869,#1798) ;
#1416 = LINE('',#9871,#1799) ;
#1417 = LINE('',#9934,#1800) ;
#1418 = LINE('',#9935,#1801) ;
#1419 = LINE('',#9943,#1802) ;
#1420 = LINE('',#9944,#1803) ;
#1421 = LINE('',#9966,#1804) ;
#1422 = LINE('',#9968,#1805) ;
#1423 = LINE('',#10004,#1806) ;
#1424 = LINE('',#10006,#1807) ;
#1425 = LINE('',#10024,#1808) ;
#1426 = LINE('',#10027,#1809) ;
#1427 = LINE('',#10030,#1810) ;
#1428 = LINE('',#10031,#1811) ;
#1429 = LINE('',#10034,#1812) ;
#1430 = LINE('',#10038,#1813) ;
#1431 = LINE('',#10039,#1814) ;
#1432 = LINE('',#10042,#1815) ;
#1433 = LINE('',#10046,#1816) ;
#1434 = LINE('',#10047,#1817) ;
#1435 = LINE('',#10050,#1818) ;
#1436 = LINE('',#10054,#1819) ;
#1437 = LINE('',#10058,#1820) ;
#1438 = LINE('',#10059,#1821) ;
#1439 = LINE('',#10062,#1822) ;
#1440 = LINE('',#10066,#1823) ;
#1441 = LINE('',#10067,#1824) ;
#1442 = LINE('',#10070,#1825) ;
#1443 = LINE('',#10074,#1826) ;
#1444 = LINE('',#10078,#1827) ;
#1445 = LINE('',#10079,#1828) ;
#1446 = LINE('',#10082,#1829) ;
#1447 = LINE('',#10087,#1830) ;
#1448 = LINE('',#10091,#1831) ;
#1449 = LINE('',#10125,#1832) ;
#1450 = LINE('',#10141,#1833) ;
#1451 = LINE('',#10161,#1834) ;
#1452 = LINE('',#10175,#1835) ;
#1453 = LINE('',#10221,#1836) ;
#1454 = LINE('',#10269,#1837) ;
#1455 = LINE('',#10271,#1838) ;
#1456 = LINE('',#10333,#1839) ;
#1457 = LINE('',#10336,#1840) ;
#1458 = LINE('',#10395,#1841) ;
#1459 = LINE('',#10396,#1842) ;
#1460 = LINE('',#10399,#1843) ;
#1461 = LINE('',#10458,#1844) ;
#1462 = LINE('',#10459,#1845) ;
#1463 = LINE('',#10476,#1846) ;
#1464 = LINE('',#10505,#1847) ;
#1465 = LINE('',#10506,#1848) ;
#1466 = LINE('',#10524,#1849) ;
#1467 = LINE('',#10538,#1850) ;
#1468 = LINE('',#10559,#1851) ;
#1469 = LINE('',#10589,#1852) ;
#1470 = LINE('',#10626,#1853) ;
#1471 = LINE('',#10628,#1854) ;
#1472 = LINE('',#10630,#1855) ;
#1473 = LINE('',#10632,#1856) ;
#1474 = LINE('',#10634,#1857) ;
#1475 = LINE('',#10636,#1858) ;
#1476 = LINE('',#10638,#1859) ;
#1477 = LINE('',#10640,#1860) ;
#1478 = LINE('',#10642,#1861) ;
#1479 = LINE('',#10644,#1862) ;
#1480 = LINE('',#10646,#1863) ;
#1481 = LINE('',#10648,#1864) ;
#1482 = LINE('',#10650,#1865) ;
#1483 = LINE('',#10652,#1866) ;
#1484 = LINE('',#10659,#1867) ;
#1485 = LINE('',#10662,#1868) ;
#1486 = LINE('',#10680,#1869) ;
#1487 = LINE('',#10722,#1870) ;
#1488 = LINE('',#10727,#1871) ;
#1489 = LINE('',#10730,#1872) ;
#1490 = LINE('',#10733,#1873) ;
#1491 = LINE('',#10734,#1874) ;
#1492 = LINE('',#10788,#1875) ;
#1493 = LINE('',#10791,#1876) ;
#1494 = LINE('',#10793,#1877) ;
#1495 = LINE('',#10802,#1878) ;
#1496 = LINE('',#10806,#1879) ;
#1497 = LINE('',#10810,#1880) ;
#1498 = LINE('',#10819,#1881) ;
#1499 = LINE('',#10826,#1882) ;
#1500 = LINE('',#10830,#1883) ;
#1501 = LINE('',#10834,#1884) ;
#1502 = LINE('',#10841,#1885) ;
#1503 = LINE('',#10850,#1886) ;
#1504 = LINE('',#10854,#1887) ;
#1505 = LINE('',#10858,#1888) ;
#1506 = LINE('',#10865,#1889) ;
#1507 = LINE('',#10870,#1890) ;
#1508 = LINE('',#10872,#1891) ;
#1509 = LINE('',#10874,#1892) ;
#1510 = LINE('',#10875,#1893) ;
#1511 = LINE('',#10878,#1894) ;
#1512 = LINE('',#10880,#1895) ;
#1513 = LINE('',#10881,#1896) ;
#1514 = LINE('',#10884,#1897) ;
#1515 = LINE('',#10886,#1898) ;
#1516 = LINE('',#10887,#1899) ;
#1517 = LINE('',#10890,#1900) ;
#1518 = LINE('',#10892,#1901) ;
#1519 = LINE('',#10893,#1902) ;
#1520 = LINE('',#10896,#1903) ;
#1521 = LINE('',#10898,#1904) ;
#1522 = LINE('',#10899,#1905) ;
#1523 = LINE('',#10902,#1906) ;
#1524 = LINE('',#10904,#1907) ;
#1525 = LINE('',#10905,#1908) ;
#1526 = LINE('',#10908,#1909) ;
#1527 = LINE('',#10910,#1910) ;
#1528 = LINE('',#10911,#1911) ;
#1529 = LINE('',#10914,#1912) ;
#1530 = LINE('',#10916,#1913) ;
#1531 = LINE('',#10917,#1914) ;
#1532 = LINE('',#10919,#1915) ;
#1533 = LINE('',#10920,#1916) ;
#1534 = LINE('',#10927,#1917) ;
#1535 = LINE('',#10929,#1918) ;
#1536 = LINE('',#10931,#1919) ;
#1537 = LINE('',#10932,#1920) ;
#1538 = LINE('',#10935,#1921) ;
#1539 = LINE('',#10937,#1922) ;
#1540 = LINE('',#10938,#1923) ;
#1541 = LINE('',#10941,#1924) ;
#1542 = LINE('',#10943,#1925) ;
#1543 = LINE('',#10944,#1926) ;
#1544 = LINE('',#10947,#1927) ;
#1545 = LINE('',#10949,#1928) ;
#1546 = LINE('',#10950,#1929) ;
#1547 = LINE('',#10953,#1930) ;
#1548 = LINE('',#10955,#1931) ;
#1549 = LINE('',#10956,#1932) ;
#1550 = LINE('',#10958,#1933) ;
#1551 = LINE('',#10959,#1934) ;
#1552 = LINE('',#10967,#1935) ;
#1553 = LINE('',#10971,#1936) ;
#1554 = LINE('',#10975,#1937) ;
#1555 = LINE('',#10979,#1938) ;
#1556 = LINE('',#10983,#1939) ;
#1557 = LINE('',#10990,#1940) ;
#1558 = LINE('',#11078,#1941) ;
#1559 = LINE('',#11125,#1942) ;
#1560 = LINE('',#11155,#1943) ;
#1561 = LINE('',#11167,#1944) ;
#1562 = LINE('',#11175,#1945) ;
#1563 = LINE('',#11182,#1946) ;
#1564 = LINE('',#11190,#1947) ;
#1565 = LINE('',#11197,#1948) ;
#1566 = LINE('',#11205,#1949) ;
#1567 = LINE('',#11213,#1950) ;
#1568 = LINE('',#11216,#1951) ;
#1569 = LINE('',#11219,#1952) ;
#1570 = LINE('',#11221,#1953) ;
#1571 = LINE('',#11222,#1954) ;
#1572 = LINE('',#11225,#1955) ;
#1573 = LINE('',#11227,#1956) ;
#1574 = LINE('',#11228,#1957) ;
#1575 = LINE('',#11234,#1958) ;
#1576 = LINE('',#11237,#1959) ;
#1577 = LINE('',#11239,#1960) ;
#1578 = LINE('',#11240,#1961) ;
#1579 = LINE('',#11246,#1962) ;
#1580 = LINE('',#11252,#1963) ;
#1581 = LINE('',#11254,#1964) ;
#1582 = LINE('',#11255,#1965) ;
#1583 = LINE('',#11263,#1966) ;
#1584 = LINE('',#11270,#1967) ;
#1585 = LINE('',#11273,#1968) ;
#1586 = LINE('',#11276,#1969) ;
#1587 = LINE('',#11278,#1970) ;
#1588 = LINE('',#11279,#1971) ;
#1589 = LINE('',#11285,#1972) ;
#1590 = LINE('',#11291,#1973) ;
#1591 = LINE('',#11294,#1974) ;
#1592 = LINE('',#11296,#1975) ;
#1593 = LINE('',#11297,#1976) ;
#1594 = LINE('',#11303,#1977) ;
#1595 = LINE('',#11306,#1978) ;
#1596 = LINE('',#11308,#1979) ;
#1597 = LINE('',#11309,#1980) ;
#1598 = LINE('',#11315,#1981) ;
#1599 = LINE('',#11321,#1982) ;
#1600 = LINE('',#11323,#1983) ;
#1601 = LINE('',#11324,#1984) ;
#1602 = LINE('',#11332,#1985) ;
#1603 = LINE('',#11340,#1986) ;
#1604 = VECTOR('',#6423,1.75) ;
#1605 = VECTOR('',#6430,3.98) ;
#1606 = VECTOR('',#6437,3.98) ;
#1607 = VECTOR('',#6444,10.) ;
#1608 = VECTOR('',#6445,10.) ;
#1609 = VECTOR('',#6446,10.) ;
#1610 = VECTOR('',#6449,10.) ;
#1611 = VECTOR('',#6452,10.) ;
#1612 = VECTOR('',#6453,10.) ;
#1613 = VECTOR('',#6454,10.) ;
#1614 = VECTOR('',#6455,10.) ;
#1615 = VECTOR('',#6456,10.) ;
#1616 = VECTOR('',#6457,10.) ;
#1617 = VECTOR('',#6458,10.) ;
#1618 = VECTOR('',#6461,10.) ;
#1619 = VECTOR('',#6462,10.) ;
#1620 = VECTOR('',#6465,10.) ;
#1621 = VECTOR('',#6466,10.) ;
#1622 = VECTOR('',#6469,10.) ;
#1623 = VECTOR('',#6470,10.) ;
#1624 = VECTOR('',#6473,10.) ;
#1625 = VECTOR('',#6474,10.) ;
#1626 = VECTOR('',#6477,10.) ;
#1627 = VECTOR('',#6478,10.) ;
#1628 = VECTOR('',#6479,10.) ;
#1629 = VECTOR('',#6482,10.) ;
#1630 = VECTOR('',#6483,10.) ;
#1631 = VECTOR('',#6484,10.) ;
#1632 = VECTOR('',#6491,10.) ;
#1633 = VECTOR('',#6496,10.) ;
#1634 = VECTOR('',#6511,10.) ;
#1635 = VECTOR('',#6512,10.) ;
#1636 = VECTOR('',#6523,10.) ;
#1637 = VECTOR('',#6524,10.) ;
#1638 = VECTOR('',#6527,10.) ;
#1639 = VECTOR('',#6528,10.) ;
#1640 = VECTOR('',#6529,10.) ;
#1641 = VECTOR('',#6532,10.) ;
#1642 = VECTOR('',#6539,10.) ;
#1643 = VECTOR('',#6542,10.) ;
#1644 = VECTOR('',#6543,10.) ;
#1645 = VECTOR('',#6544,10.) ;
#1646 = VECTOR('',#6557,2.665) ;
#1647 = VECTOR('',#6572,10.) ;
#1648 = VECTOR('',#6573,10.) ;
#1649 = VECTOR('',#6576,10.) ;
#1650 = VECTOR('',#6579,10.) ;
#1651 = VECTOR('',#6582,10.) ;
#1652 = VECTOR('',#6585,10.) ;
#1653 = VECTOR('',#6588,2.665) ;
#1654 = VECTOR('',#6603,10.) ;
#1655 = VECTOR('',#6612,10.) ;
#1656 = VECTOR('',#6615,10.) ;
#1657 = VECTOR('',#6616,10.) ;
#1658 = VECTOR('',#6617,10.) ;
#1659 = VECTOR('',#6620,10.) ;
#1660 = VECTOR('',#6631,10.) ;
#1661 = VECTOR('',#6632,10.) ;
#1662 = VECTOR('',#6637,10.) ;
#1663 = VECTOR('',#6656,10.) ;
#1664 = VECTOR('',#6681,10.) ;
#1665 = VECTOR('',#6684,10.) ;
#1666 = VECTOR('',#6691,10.) ;
#1667 = VECTOR('',#6696,10.) ;
#1668 = VECTOR('',#6711,10.) ;
#1669 = VECTOR('',#6712,10.) ;
#1670 = VECTOR('',#6727,10.) ;
#1671 = VECTOR('',#6728,10.) ;
#1672 = VECTOR('',#6729,10.) ;
#1673 = VECTOR('',#6732,10.) ;
#1674 = VECTOR('',#6739,10.) ;
#1675 = VECTOR('',#6744,10.) ;
#1676 = VECTOR('',#6747,10.) ;
#1677 = VECTOR('',#6750,10.) ;
#1678 = VECTOR('',#6751,10.) ;
#1679 = VECTOR('',#6754,10.) ;
#1680 = VECTOR('',#6755,10.) ;
#1681 = VECTOR('',#6768,10.) ;
#1682 = VECTOR('',#6773,10.) ;
#1683 = VECTOR('',#6776,10.) ;
#1684 = VECTOR('',#6779,10.) ;
#1685 = VECTOR('',#6780,10.) ;
#1686 = VECTOR('',#6783,10.) ;
#1687 = VECTOR('',#6788,10.) ;
#1688 = VECTOR('',#6789,10.) ;
#1689 = VECTOR('',#6792,10.) ;
#1690 = VECTOR('',#6805,10.) ;
#1691 = VECTOR('',#6806,10.) ;
#1692 = VECTOR('',#6813,10.) ;
#1693 = VECTOR('',#6814,10.) ;
#1694 = VECTOR('',#6821,10.) ;
#1695 = VECTOR('',#6822,10.) ;
#1696 = VECTOR('',#6823,10.) ;
#1697 = VECTOR('',#6826,10.) ;
#1698 = VECTOR('',#6831,10.) ;
#1699 = VECTOR('',#6832,10.) ;
#1700 = VECTOR('',#6835,10.) ;
#1701 = VECTOR('',#6840,10.) ;
#1702 = VECTOR('',#6841,10.) ;
#1703 = VECTOR('',#6844,10.) ;
#1704 = VECTOR('',#6849,10.) ;
#1705 = VECTOR('',#6850,10.) ;
#1706 = VECTOR('',#6853,10.) ;
#1707 = VECTOR('',#6858,10.) ;
#1708 = VECTOR('',#6859,10.) ;
#1709 = VECTOR('',#6870,10.) ;
#1710 = VECTOR('',#6873,10.) ;
#1711 = VECTOR('',#6886,10.) ;
#1712 = VECTOR('',#6889,10.) ;
#1713 = VECTOR('',#6904,10.) ;
#1714 = VECTOR('',#6905,10.) ;
#1715 = VECTOR('',#6908,10.) ;
#1716 = VECTOR('',#6911,10.) ;
#1717 = VECTOR('',#6930,10.) ;
#1718 = VECTOR('',#6931,10.) ;
#1719 = VECTOR('',#6942,10.) ;
#1720 = VECTOR('',#6943,10.) ;
#1721 = VECTOR('',#6946,10.) ;
#1722 = VECTOR('',#6947,10.) ;
#1723 = VECTOR('',#6948,10.) ;
#1724 = VECTOR('',#6951,10.) ;
#1725 = VECTOR('',#6956,10.) ;
#1726 = VECTOR('',#6959,10.) ;
#1727 = VECTOR('',#6966,10.) ;
#1728 = VECTOR('',#6969,10.) ;
#1729 = VECTOR('',#6970,10.) ;
#1730 = VECTOR('',#6973,10.) ;
#1731 = VECTOR('',#6976,10.) ;
#1732 = VECTOR('',#6989,10.) ;
#1733 = VECTOR('',#6998,10.) ;
#1734 = VECTOR('',#7001,10.) ;
#1735 = VECTOR('',#7002,10.) ;
#1736 = VECTOR('',#7003,10.) ;
#1737 = VECTOR('',#7006,10.) ;
#1738 = VECTOR('',#7011,10.) ;
#1739 = VECTOR('',#7014,10.) ;
#1740 = VECTOR('',#7021,10.) ;
#1741 = VECTOR('',#7032,10.) ;
#1742 = VECTOR('',#7045,10.) ;
#1743 = VECTOR('',#7056,10.) ;
#1744 = VECTOR('',#7059,10.) ;
#1745 = VECTOR('',#7060,10.) ;
#1746 = VECTOR('',#7061,10.) ;
#1747 = VECTOR('',#7062,10.) ;
#1748 = VECTOR('',#7065,10.) ;
#1749 = VECTOR('',#7070,10.) ;
#1750 = VECTOR('',#7071,10.) ;
#1751 = VECTOR('',#7074,10.) ;
#1752 = VECTOR('',#7079,10.) ;
#1753 = VECTOR('',#7084,10.) ;
#1754 = VECTOR('',#7089,10.) ;
#1755 = VECTOR('',#7090,10.) ;
#1756 = VECTOR('',#7093,10.) ;
#1757 = VECTOR('',#7098,10.) ;
#1758 = VECTOR('',#7099,10.) ;
#1759 = VECTOR('',#7100,10.) ;
#1760 = VECTOR('',#7103,1.585) ;
#1761 = VECTOR('',#7110,1.585) ;
#1762 = VECTOR('',#7113,10.) ;
#1763 = VECTOR('',#7114,10.) ;
#1764 = VECTOR('',#7115,10.) ;
#1765 = VECTOR('',#7118,10.) ;
#1766 = VECTOR('',#7123,10.) ;
#1767 = VECTOR('',#7124,10.) ;
#1768 = VECTOR('',#7125,10.) ;
#1769 = VECTOR('',#7128,10.) ;
#1770 = VECTOR('',#7129,10.) ;
#1771 = VECTOR('',#7134,10.) ;
#1772 = VECTOR('',#7137,10.) ;
#1773 = VECTOR('',#7138,10.) ;
#1774 = VECTOR('',#7143,10.) ;
#1775 = VECTOR('',#7146,10.) ;
#1776 = VECTOR('',#7149,10.) ;
#1777 = VECTOR('',#7154,10.) ;
#1778 = VECTOR('',#7159,10.) ;
#1779 = VECTOR('',#7164,10.) ;
#1780 = VECTOR('',#7171,10.) ;
#1781 = VECTOR('',#7172,10.) ;
#1782 = VECTOR('',#7179,10.) ;
#1783 = VECTOR('',#7180,10.) ;
#1784 = VECTOR('',#7189,10.) ;
#1785 = VECTOR('',#7190,10.) ;
#1786 = VECTOR('',#7199,10.) ;
#1787 = VECTOR('',#7200,10.) ;
#1788 = VECTOR('',#7209,10.) ;
#1789 = VECTOR('',#7210,10.) ;
#1790 = VECTOR('',#7219,10.) ;
#1791 = VECTOR('',#7220,10.) ;
#1792 = VECTOR('',#7223,10.) ;
#1793 = VECTOR('',#7224,10.) ;
#1794 = VECTOR('',#7255,10.) ;
#1795 = VECTOR('',#7256,10.) ;
#1796 = VECTOR('',#7259,10.) ;
#1797 = VECTOR('',#7260,10.) ;
#1798 = VECTOR('',#7263,10.) ;
#1799 = VECTOR('',#7264,10.) ;
#1800 = VECTOR('',#7279,10.) ;
#1801 = VECTOR('',#7280,10.) ;
#1802 = VECTOR('',#7291,10.) ;
#1803 = VECTOR('',#7292,10.) ;
#1804 = VECTOR('',#7301,10.) ;
#1805 = VECTOR('',#7302,10.) ;
#1806 = VECTOR('',#7311,10.) ;
#1807 = VECTOR('',#7312,10.) ;
#1808 = VECTOR('',#7321,10.) ;
#1809 = VECTOR('',#7324,10.) ;
#1810 = VECTOR('',#7327,10.) ;
#1811 = VECTOR('',#7328,10.) ;
#1812 = VECTOR('',#7331,10.) ;
#1813 = VECTOR('',#7336,10.) ;
#1814 = VECTOR('',#7337,10.) ;
#1815 = VECTOR('',#7340,10.) ;
#1816 = VECTOR('',#7345,10.) ;
#1817 = VECTOR('',#7346,10.) ;
#1818 = VECTOR('',#7349,10.) ;
#1819 = VECTOR('',#7354,10.) ;
#1820 = VECTOR('',#7359,10.) ;
#1821 = VECTOR('',#7360,10.) ;
#1822 = VECTOR('',#7363,10.) ;
#1823 = VECTOR('',#7368,10.) ;
#1824 = VECTOR('',#7369,10.) ;
#1825 = VECTOR('',#7372,10.) ;
#1826 = VECTOR('',#7377,10.) ;
#1827 = VECTOR('',#7382,10.) ;
#1828 = VECTOR('',#7383,10.) ;
#1829 = VECTOR('',#7386,10.) ;
#1830 = VECTOR('',#7391,10.) ;
#1831 = VECTOR('',#7394,10.) ;
#1832 = VECTOR('',#7405,10.) ;
#1833 = VECTOR('',#7406,10.) ;
#1834 = VECTOR('',#7415,10.) ;
#1835 = VECTOR('',#7416,10.) ;
#1836 = VECTOR('',#7425,10.) ;
#1837 = VECTOR('',#7436,10.) ;
#1838 = VECTOR('',#7437,10.) ;
#1839 = VECTOR('',#7450,10.) ;
#1840 = VECTOR('',#7453,10.) ;
#1841 = VECTOR('',#7462,10.) ;
#1842 = VECTOR('',#7463,10.) ;
#1843 = VECTOR('',#7466,10.) ;
#1844 = VECTOR('',#7479,10.) ;
#1845 = VECTOR('',#7480,10.) ;
#1846 = VECTOR('',#7487,10.) ;
#1847 = VECTOR('',#7490,10.) ;
#1848 = VECTOR('',#7491,10.) ;
#1849 = VECTOR('',#7498,10.) ;
#1850 = VECTOR('',#7499,10.) ;
#1851 = VECTOR('',#7512,10.) ;
#1852 = VECTOR('',#7519,10.) ;
#1853 = VECTOR('',#7524,10.) ;
#1854 = VECTOR('',#7527,10.) ;
#1855 = VECTOR('',#7530,10.) ;
#1856 = VECTOR('',#7533,10.) ;
#1857 = VECTOR('',#7536,10.) ;
#1858 = VECTOR('',#7539,10.) ;
#1859 = VECTOR('',#7542,10.) ;
#1860 = VECTOR('',#7545,10.) ;
#1861 = VECTOR('',#7548,10.) ;
#1862 = VECTOR('',#7551,10.) ;
#1863 = VECTOR('',#7554,10.) ;
#1864 = VECTOR('',#7557,10.) ;
#1865 = VECTOR('',#7560,10.) ;
#1866 = VECTOR('',#7563,10.) ;
#1867 = VECTOR('',#7570,10.) ;
#1868 = VECTOR('',#7573,10.) ;
#1869 = VECTOR('',#7578,10.) ;
#1870 = VECTOR('',#7585,10.) ;
#1871 = VECTOR('',#7592,10.) ;
#1872 = VECTOR('',#7595,10.) ;
#1873 = VECTOR('',#7598,10.) ;
#1874 = VECTOR('',#7599,10.) ;
#1875 = VECTOR('',#7608,10.) ;
#1876 = VECTOR('',#7613,3.97) ;
#1877 = VECTOR('',#7616,10.) ;
#1878 = VECTOR('',#7629,3.825) ;
#1879 = VECTOR('',#7634,3.95) ;
#1880 = VECTOR('',#7639,3.825) ;
#1881 = VECTOR('',#7652,1.5) ;
#1882 = VECTOR('',#7661,5.05) ;
#1883 = VECTOR('',#7666,5.175) ;
#1884 = VECTOR('',#7671,5.05) ;
#1885 = VECTOR('',#7680,1.5) ;
#1886 = VECTOR('',#7693,1.525) ;
#1887 = VECTOR('',#7698,1.65) ;
#1888 = VECTOR('',#7703,1.525) ;
#1889 = VECTOR('',#7712,1.7) ;
#1890 = VECTOR('',#7717,10.) ;
#1891 = VECTOR('',#7718,10.) ;
#1892 = VECTOR('',#7719,10.) ;
#1893 = VECTOR('',#7720,10.) ;
#1894 = VECTOR('',#7723,10.) ;
#1895 = VECTOR('',#7724,10.) ;
#1896 = VECTOR('',#7725,10.) ;
#1897 = VECTOR('',#7728,10.) ;
#1898 = VECTOR('',#7729,10.) ;
#1899 = VECTOR('',#7730,10.) ;
#1900 = VECTOR('',#7733,10.) ;
#1901 = VECTOR('',#7734,10.) ;
#1902 = VECTOR('',#7735,10.) ;
#1903 = VECTOR('',#7738,10.) ;
#1904 = VECTOR('',#7739,10.) ;
#1905 = VECTOR('',#7740,10.) ;
#1906 = VECTOR('',#7743,10.) ;
#1907 = VECTOR('',#7744,10.) ;
#1908 = VECTOR('',#7745,10.) ;
#1909 = VECTOR('',#7748,10.) ;
#1910 = VECTOR('',#7749,10.) ;
#1911 = VECTOR('',#7750,10.) ;
#1912 = VECTOR('',#7753,10.) ;
#1913 = VECTOR('',#7754,10.) ;
#1914 = VECTOR('',#7755,10.) ;
#1915 = VECTOR('',#7758,10.) ;
#1916 = VECTOR('',#7759,10.) ;
#1917 = VECTOR('',#7768,10.) ;
#1918 = VECTOR('',#7769,10.) ;
#1919 = VECTOR('',#7770,10.) ;
#1920 = VECTOR('',#7771,10.) ;
#1921 = VECTOR('',#7774,10.) ;
#1922 = VECTOR('',#7775,10.) ;
#1923 = VECTOR('',#7776,10.) ;
#1924 = VECTOR('',#7779,10.) ;
#1925 = VECTOR('',#7780,10.) ;
#1926 = VECTOR('',#7781,10.) ;
#1927 = VECTOR('',#7784,10.) ;
#1928 = VECTOR('',#7785,10.) ;
#1929 = VECTOR('',#7786,10.) ;
#1930 = VECTOR('',#7789,10.) ;
#1931 = VECTOR('',#7790,10.) ;
#1932 = VECTOR('',#7791,10.) ;
#1933 = VECTOR('',#7794,10.) ;
#1934 = VECTOR('',#7795,10.) ;
#1935 = VECTOR('',#7806,1.80518500301908) ;
#1936 = VECTOR('',#7811,1.90519525249383) ;
#1937 = VECTOR('',#7816,1.76268064699232) ;
#1938 = VECTOR('',#7821,1.62016604149081) ;
#1939 = VECTOR('',#7826,1.56015989180597) ;
#1940 = VECTOR('',#7835,0.605) ;
#1941 = VECTOR('',#7838,0.605) ;
#1942 = VECTOR('',#7861,0.605) ;
#1943 = VECTOR('',#7866,0.605) ;
#1944 = VECTOR('',#7883,3.985) ;
#1945 = VECTOR('',#7894,6.105) ;
#1946 = VECTOR('',#7903,3.985) ;
#1947 = VECTOR('',#7914,5.4) ;
#1948 = VECTOR('',#7923,3.985) ;
#1949 = VECTOR('',#7934,5.595) ;
#1950 = VECTOR('',#7943,10.) ;
#1951 = VECTOR('',#7946,10.) ;
#1952 = VECTOR('',#7949,10.) ;
#1953 = VECTOR('',#7950,10.) ;
#1954 = VECTOR('',#7951,10.) ;
#1955 = VECTOR('',#7954,10.) ;
#1956 = VECTOR('',#7955,10.) ;
#1957 = VECTOR('',#7956,10.) ;
#1958 = VECTOR('',#7963,10.) ;
#1959 = VECTOR('',#7966,10.) ;
#1960 = VECTOR('',#7967,10.) ;
#1961 = VECTOR('',#7968,10.) ;
#1962 = VECTOR('',#7975,10.) ;
#1963 = VECTOR('',#7982,10.) ;
#1964 = VECTOR('',#7985,10.) ;
#1965 = VECTOR('',#7986,10.) ;
#1966 = VECTOR('',#7997,3.97) ;
#1967 = VECTOR('',#8004,10.) ;
#1968 = VECTOR('',#8007,10.) ;
#1969 = VECTOR('',#8010,10.) ;
#1970 = VECTOR('',#8011,10.) ;
#1971 = VECTOR('',#8012,10.) ;
#1972 = VECTOR('',#8019,10.) ;
#1973 = VECTOR('',#8026,10.) ;
#1974 = VECTOR('',#8029,10.) ;
#1975 = VECTOR('',#8030,10.) ;
#1976 = VECTOR('',#8031,10.) ;
#1977 = VECTOR('',#8038,10.) ;
#1978 = VECTOR('',#8041,10.) ;
#1979 = VECTOR('',#8042,10.) ;
#1980 = VECTOR('',#8043,10.) ;
#1981 = VECTOR('',#8050,10.) ;
#1982 = VECTOR('',#8057,10.) ;
#1983 = VECTOR('',#8060,10.) ;
#1984 = VECTOR('',#8061,10.) ;
#1985 = VECTOR('',#8072,1.525) ;
#1986 = VECTOR('',#8083,2.225) ;
#1987 = CIRCLE('',#5753,1.75) ;
#1988 = CIRCLE('',#5754,1.75) ;
#1989 = CIRCLE('',#5756,3.98) ;
#1990 = CIRCLE('',#5757,3.98) ;
#1991 = CIRCLE('',#5759,3.98) ;
#1992 = CIRCLE('',#5760,3.98) ;
#1993 = CIRCLE('',#5777,0.25) ;
#1994 = CIRCLE('',#5778,2.665) ;
#1995 = CIRCLE('',#5779,0.25) ;
#1996 = CIRCLE('',#5780,2.915) ;
#1997 = CIRCLE('',#5782,0.25) ;
#1998 = CIRCLE('',#5784,0.249999999999999) ;
#1999 = CIRCLE('',#5785,2.915) ;
#2000 = CIRCLE('',#5786,2.665) ;
#2001 = CIRCLE('',#5790,2.665) ;
#2002 = CIRCLE('',#5792,16.3358074534161) ;
#2003 = CIRCLE('',#5793,2.83595375255767) ;
#2004 = CIRCLE('',#5794,2.915) ;
#2005 = CIRCLE('',#5796,0.25) ;
#2006 = CIRCLE('',#5797,2.665) ;
#2007 = CIRCLE('',#5798,2.665) ;
#2008 = CIRCLE('',#5800,2.665) ;
#2009 = CIRCLE('',#5802,2.915) ;
#2010 = CIRCLE('',#5803,0.25) ;
#2011 = CIRCLE('',#5804,2.665) ;
#2012 = CIRCLE('',#5805,2.665) ;
#2013 = CIRCLE('',#5807,3.05499364382027) ;
#2014 = CIRCLE('',#5808,16.3358074534161) ;
#2015 = CIRCLE('',#5809,2.915) ;
#2016 = CIRCLE('',#5810,2.915) ;
#2017 = CIRCLE('',#5812,2.665) ;
#2018 = CIRCLE('',#5814,0.25) ;
#2019 = CIRCLE('',#5815,2.665) ;
#2020 = CIRCLE('',#5816,0.25) ;
#2021 = CIRCLE('',#5818,0.25) ;
#2022 = CIRCLE('',#5820,0.249999999999999) ;
#2023 = CIRCLE('',#5821,2.665) ;
#2024 = CIRCLE('',#5825,2.665) ;
#2025 = CIRCLE('',#5827,0.249999999999999) ;
#2026 = CIRCLE('',#5829,0.249999999999999) ;
#2027 = CIRCLE('',#5831,0.25) ;
#2028 = CIRCLE('',#5832,0.249999999999999) ;
#2029 = CIRCLE('',#5834,1.27) ;
#2030 = CIRCLE('',#5835,1.52) ;
#2031 = CIRCLE('',#5837,3.30499364382027) ;
#2032 = CIRCLE('',#5839,3.08595375255767) ;
#2033 = CIRCLE('',#5841,0.25) ;
#2034 = CIRCLE('',#5842,0.25) ;
#2035 = CIRCLE('',#5844,0.25) ;
#2036 = CIRCLE('',#5845,16.5858074534161) ;
#2037 = CIRCLE('',#5846,16.3358074534161) ;
#2038 = CIRCLE('',#5848,0.25) ;
#2039 = CIRCLE('',#5849,16.5858074534161) ;
#2040 = CIRCLE('',#5851,16.5858074534161) ;
#2041 = CIRCLE('',#5854,0.249999999999999) ;
#2042 = CIRCLE('',#5856,0.25) ;
#2043 = CIRCLE('',#5858,0.25) ;
#2044 = CIRCLE('',#5859,0.249999999999999) ;
#2045 = CIRCLE('',#5861,0.249999999999999) ;
#2046 = CIRCLE('',#5862,1.27) ;
#2047 = CIRCLE('',#5863,1.52) ;
#2048 = CIRCLE('',#5865,0.249999999999999) ;
#2049 = CIRCLE('',#5869,0.249999999999995) ;
#2050 = CIRCLE('',#5871,0.249999999999995) ;
#2051 = CIRCLE('',#5873,10.1848235398934) ;
#2052 = CIRCLE('',#5881,10.1848235398934) ;
#2053 = CIRCLE('',#5886,13.3598235398934) ;
#2054 = CIRCLE('',#5893,13.3598235398934) ;
#2055 = CIRCLE('',#5903,2.665) ;
#2056 = CIRCLE('',#5906,2.665) ;
#2057 = CIRCLE('',#5909,3.08595375255767) ;
#2058 = CIRCLE('',#5912,16.5858074534161) ;
#2059 = CIRCLE('',#5915,3.30499364382027) ;
#2060 = CIRCLE('',#5918,0.249999999999995) ;
#2061 = CIRCLE('',#5921,0.249999999999995) ;
#2062 = CIRCLE('',#5925,0.25) ;
#2063 = CIRCLE('',#5928,0.25) ;
#2064 = CIRCLE('',#5929,0.5) ;
#2065 = CIRCLE('',#5931,1.48867477559092) ;
#2066 = CIRCLE('',#5932,5.66550083849775) ;
#2067 = CIRCLE('',#5933,1.585) ;
#2068 = CIRCLE('',#5935,0.25) ;
#2069 = CIRCLE('',#5936,0.25) ;
#2070 = CIRCLE('',#5937,0.5) ;
#2071 = CIRCLE('',#5941,5.66550083849775) ;
#2072 = CIRCLE('',#5942,1.48867477559092) ;
#2073 = CIRCLE('',#5943,1.585) ;
#2074 = CIRCLE('',#5945,0.25) ;
#2075 = CIRCLE('',#5946,2.665) ;
#2076 = CIRCLE('',#5947,0.250000000000004) ;
#2077 = CIRCLE('',#5948,2.915) ;
#2078 = CIRCLE('',#5950,0.250000000000004) ;
#2079 = CIRCLE('',#5952,0.250000000000004) ;
#2080 = CIRCLE('',#5953,2.915) ;
#2081 = CIRCLE('',#5954,2.665) ;
#2082 = CIRCLE('',#5958,2.665) ;
#2083 = CIRCLE('',#5960,0.400000000000004) ;
#2084 = CIRCLE('',#5961,6.2066222212067) ;
#2085 = CIRCLE('',#5962,46.8573015873016) ;
#2086 = CIRCLE('',#5963,5.95626157119474) ;
#2087 = CIRCLE('',#5964,0.399999999999999) ;
#2088 = CIRCLE('',#5965,2.915) ;
#2089 = CIRCLE('',#5966,2.915) ;
#2090 = CIRCLE('',#5968,0.25) ;
#2091 = CIRCLE('',#5969,2.665) ;
#2092 = CIRCLE('',#5970,0.250000000000004) ;
#2093 = CIRCLE('',#5972,0.250000000000004) ;
#2094 = CIRCLE('',#5974,0.250000000000004) ;
#2095 = CIRCLE('',#5975,2.665) ;
#2096 = CIRCLE('',#5979,2.665) ;
#2097 = CIRCLE('',#5983,6.20626157119474) ;
#2098 = CIRCLE('',#5985,0.249999999999999) ;
#2099 = CIRCLE('',#5987,0.250000000000004) ;
#2100 = CIRCLE('',#5988,0.649999999999999) ;
#2101 = CIRCLE('',#5991,6.4566222212067) ;
#2102 = CIRCLE('',#5992,0.249999999999994) ;
#2103 = CIRCLE('',#5994,47.1073015873016) ;
#2104 = CIRCLE('',#5996,0.249999999999999) ;
#2105 = CIRCLE('',#5998,0.249999999999999) ;
#2106 = CIRCLE('',#5999,0.650000000000004) ;
#2107 = CIRCLE('',#6003,0.649999999999999) ;
#2108 = CIRCLE('',#6006,6.20626157119473) ;
#2109 = CIRCLE('',#6008,47.1073015873016) ;
#2110 = CIRCLE('',#6010,6.4566222212067) ;
#2111 = CIRCLE('',#6013,0.650000000000004) ;
#2112 = CIRCLE('',#6016,1.585) ;
#2113 = CIRCLE('',#6018,1.585) ;
#2114 = CIRCLE('',#6020,5.45) ;
#2115 = CIRCLE('',#6021,5.66550083849775) ;
#2116 = CIRCLE('',#6025,5.45) ;
#2117 = CIRCLE('',#6028,5.66550083849775) ;
#2118 = CIRCLE('',#6030,2.665) ;
#2119 = CIRCLE('',#6031,2.665) ;
#2120 = CIRCLE('',#6040,0.132505429325631) ;
#2121 = CIRCLE('',#6041,0.332505429325631) ;
#2122 = CIRCLE('',#6044,5.6095419988581) ;
#2123 = CIRCLE('',#6045,5.4095419988581) ;
#2124 = CIRCLE('',#6048,18.7717409779691) ;
#2125 = CIRCLE('',#6049,18.9717409779691) ;
#2126 = CIRCLE('',#6052,6.02789861439302) ;
#2127 = CIRCLE('',#6053,6.22789861439302) ;
#2128 = CIRCLE('',#6056,0.524935224963979) ;
#2129 = CIRCLE('',#6057,0.324935224963979) ;
#2130 = CIRCLE('',#6062,1.8962519345458) ;
#2131 = CIRCLE('',#6063,1.6962519345458) ;
#2132 = CIRCLE('',#6065,20.767808830506) ;
#2133 = CIRCLE('',#6066,20.567808830506) ;
#2134 = CIRCLE('',#6068,6.24675996480777) ;
#2135 = CIRCLE('',#6069,6.44675996480776) ;
#2136 = CIRCLE('',#6071,9.77267576253889) ;
#2137 = CIRCLE('',#6072,0.2) ;
#2138 = CIRCLE('',#6073,9.57267576253889) ;
#2139 = CIRCLE('',#6078,1.00004201680672) ;
#2140 = CIRCLE('',#6079,1.20004201680672) ;
#2141 = CIRCLE('',#6081,4.43606098801213) ;
#2142 = CIRCLE('',#6082,4.23606098801213) ;
#2143 = CIRCLE('',#6085,7.93937148944777) ;
#2144 = CIRCLE('',#6086,0.199999999999997) ;
#2145 = CIRCLE('',#6087,8.13937148944777) ;
#2146 = CIRCLE('',#6090,3.76067266925812) ;
#2147 = CIRCLE('',#6091,3.96067266925812) ;
#2148 = CIRCLE('',#6094,4.37909654020415) ;
#2149 = CIRCLE('',#6095,4.17909654020415) ;
#2150 = CIRCLE('',#6098,0.474381812079108) ;
#2151 = CIRCLE('',#6099,0.274381812079108) ;
#2152 = CIRCLE('',#6101,0.474381812079108) ;
#2153 = CIRCLE('',#6104,0.332505429325631) ;
#2154 = CIRCLE('',#6107,5.4095419988581) ;
#2155 = CIRCLE('',#6110,6.22789861439302) ;
#2156 = CIRCLE('',#6112,0.324935224963979) ;
#2157 = CIRCLE('',#6115,1.20004201680672) ;
#2158 = CIRCLE('',#6118,1.6962519345458) ;
#2159 = CIRCLE('',#6120,6.44675996480776) ;
#2160 = CIRCLE('',#6123,9.57267576253889) ;
#2161 = CIRCLE('',#6125,0.85017716535433) ;
#2162 = CIRCLE('',#6126,0.85017716535433) ;
#2163 = CIRCLE('',#6127,3.97) ;
#2164 = CIRCLE('',#6129,0.274381812079108) ;
#2165 = CIRCLE('',#6132,4.37909654020415) ;
#2166 = CIRCLE('',#6133,4.17909654020415) ;
#2167 = CIRCLE('',#6136,3.96067266925812) ;
#2168 = CIRCLE('',#6137,3.76067266925812) ;
#2169 = CIRCLE('',#6140,8.13937148944777) ;
#2170 = CIRCLE('',#6141,0.2) ;
#2171 = CIRCLE('',#6142,7.93937148944777) ;
#2172 = CIRCLE('',#6145,1.00004201680672) ;
#2173 = CIRCLE('',#6147,4.23606098801213) ;
#2174 = CIRCLE('',#6148,4.43606098801213) ;
#2175 = CIRCLE('',#6152,0.2) ;
#2176 = CIRCLE('',#6153,9.77267576253889) ;
#2177 = CIRCLE('',#6157,20.567808830506) ;
#2178 = CIRCLE('',#6158,20.767808830506) ;
#2179 = CIRCLE('',#6160,6.24675996480777) ;
#2180 = CIRCLE('',#6163,1.8962519345458) ;
#2181 = CIRCLE('',#6167,0.524935224963979) ;
#2182 = CIRCLE('',#6170,18.9717409779691) ;
#2183 = CIRCLE('',#6171,18.7717409779691) ;
#2184 = CIRCLE('',#6173,6.02789861439302) ;
#2185 = CIRCLE('',#6176,5.6095419988581) ;
#2186 = CIRCLE('',#6178,0.132505429325631) ;
#2187 = CIRCLE('',#6195,0.85017716535433) ;
#2188 = CIRCLE('',#6196,0.85017716535433) ;
#2189 = CIRCLE('',#6197,3.97) ;
#2190 = CIRCLE('',#6200,0.65017716535433) ;
#2191 = CIRCLE('',#6203,0.65017716535433) ;
#2192 = CIRCLE('',#6205,0.65017716535433) ;
#2193 = CIRCLE('',#6208,0.65017716535433) ;
#2194 = CIRCLE('',#6217,3.7) ;
#2195 = CIRCLE('',#6219,3.95) ;
#2196 = CIRCLE('',#6221,3.95) ;
#2197 = CIRCLE('',#6223,3.7) ;
#2198 = CIRCLE('',#6227,1.5) ;
#2199 = CIRCLE('',#6229,1.5) ;
#2200 = CIRCLE('',#6231,4.925) ;
#2201 = CIRCLE('',#6233,5.175) ;
#2202 = CIRCLE('',#6235,5.175) ;
#2203 = CIRCLE('',#6237,4.925) ;
#2204 = CIRCLE('',#6239,1.5) ;
#2205 = CIRCLE('',#6241,1.5) ;
#2206 = CIRCLE('',#6245,1.4) ;
#2207 = CIRCLE('',#6247,1.65) ;
#2208 = CIRCLE('',#6249,1.65) ;
#2209 = CIRCLE('',#6251,1.4) ;
#2210 = CIRCLE('',#6255,1.7) ;
#2211 = CIRCLE('',#6256,1.7) ;
#2212 = CIRCLE('',#6277,1.70517475354434) ;
#2213 = CIRCLE('',#6279,1.90519525249382) ;
#2214 = CIRCLE('',#6281,1.90519525249383) ;
#2215 = CIRCLE('',#6283,1.62016604149081) ;
#2216 = CIRCLE('',#6285,1.62016604149081) ;
#2217 = CIRCLE('',#6287,1.50015374212112) ;
#2218 = CIRCLE('',#6291,0.605) ;
#2219 = CIRCLE('',#6294,4.6273791265187) ;
#2220 = CIRCLE('',#6295,0.605) ;
#2221 = CIRCLE('',#6296,4.78262087348138) ;
#2222 = CIRCLE('',#6297,4.78262087348138) ;
#2223 = CIRCLE('',#6299,0.605) ;
#2224 = CIRCLE('',#6300,4.78262087348138) ;
#2225 = CIRCLE('',#6301,4.78262087348138) ;
#2226 = CIRCLE('',#6303,0.605) ;
#2227 = CIRCLE('',#6304,0.605) ;
#2228 = CIRCLE('',#6307,4.62737912651871) ;
#2229 = CIRCLE('',#6308,0.605) ;
#2230 = CIRCLE('',#6310,0.605) ;
#2231 = CIRCLE('',#6313,3.985) ;
#2232 = CIRCLE('',#6314,3.985) ;
#2233 = CIRCLE('',#6316,6.105) ;
#2234 = CIRCLE('',#6318,6.105) ;
#2235 = CIRCLE('',#6322,3.985) ;
#2236 = CIRCLE('',#6323,3.985) ;
#2237 = CIRCLE('',#6325,5.4) ;
#2238 = CIRCLE('',#6327,5.4) ;
#2239 = CIRCLE('',#6331,3.985) ;
#2240 = CIRCLE('',#6332,3.985) ;
#2241 = CIRCLE('',#6334,5.595) ;
#2242 = CIRCLE('',#6336,5.595) ;
#2243 = CIRCLE('',#6340,2.55000000000001) ;
#2244 = CIRCLE('',#6341,2.55000000000001) ;
#2245 = CIRCLE('',#6345,4.00044834860818) ;
#2246 = CIRCLE('',#6346,4.00044834860818) ;
#2247 = CIRCLE('',#6349,13.4930018479188) ;
#2248 = CIRCLE('',#6350,13.4930018479188) ;
#2249 = CIRCLE('',#6352,1.26348906976575) ;
#2250 = CIRCLE('',#6353,1.26348906976575) ;
#2251 = CIRCLE('',#6359,3.97) ;
#2252 = CIRCLE('',#6360,3.97) ;
#2253 = CIRCLE('',#6362,2.55000000000001) ;
#2254 = CIRCLE('',#6363,2.55000000000001) ;
#2255 = CIRCLE('',#6366,1.34638068543699) ;
#2256 = CIRCLE('',#6367,1.34638068543699) ;
#2257 = CIRCLE('',#6369,13.5130476224576) ;
#2258 = CIRCLE('',#6370,13.5130476224576) ;
#2259 = CIRCLE('',#6373,1.8820937834387) ;
#2260 = CIRCLE('',#6374,1.8820937834387) ;
#2261 = CIRCLE('',#6377,13.5002427920346) ;
#2262 = CIRCLE('',#6378,13.5002427920346) ;
#2263 = CIRCLE('',#6380,1.26348906976575) ;
#2264 = CIRCLE('',#6381,1.26348906976575) ;
#2265 = CIRCLE('',#6387,1.525) ;
#2266 = CIRCLE('',#6388,1.525) ;
#2267 = CIRCLE('',#6390,2.225) ;
#2268 = CIRCLE('',#6392,2.225) ;
#2269 = VERTEX_POINT('',#8131) ;
#2270 = VERTEX_POINT('',#8133) ;
#2271 = VERTEX_POINT('',#8137) ;
#2272 = VERTEX_POINT('',#8139) ;
#2273 = VERTEX_POINT('',#8143) ;
#2274 = VERTEX_POINT('',#8145) ;
#2275 = VERTEX_POINT('',#8149) ;
#2276 = VERTEX_POINT('',#8150) ;
#2277 = VERTEX_POINT('',#8152) ;
#2278 = VERTEX_POINT('',#8154) ;
#2279 = VERTEX_POINT('',#8156) ;
#2280 = VERTEX_POINT('',#8158) ;
#2281 = VERTEX_POINT('',#8162) ;
#2282 = VERTEX_POINT('',#8164) ;
#2283 = VERTEX_POINT('',#8166) ;
#2284 = VERTEX_POINT('',#8168) ;
#2285 = VERTEX_POINT('',#8170) ;
#2286 = VERTEX_POINT('',#8172) ;
#2287 = VERTEX_POINT('',#8176) ;
#2288 = VERTEX_POINT('',#8180) ;
#2289 = VERTEX_POINT('',#8184) ;
#2290 = VERTEX_POINT('',#8188) ;
#2291 = VERTEX_POINT('',#8192) ;
#2292 = VERTEX_POINT('',#8194) ;
#2293 = VERTEX_POINT('',#8198) ;
#2294 = VERTEX_POINT('',#8200) ;
#2295 = VERTEX_POINT('',#8204) ;
#2296 = VERTEX_POINT('',#8206) ;
#2297 = VERTEX_POINT('',#8208) ;
#2298 = VERTEX_POINT('',#8212) ;
#2299 = VERTEX_POINT('',#8235) ;
#2300 = VERTEX_POINT('',#8236) ;
#2301 = VERTEX_POINT('',#8238) ;
#2302 = VERTEX_POINT('',#8240) ;
#2303 = VERTEX_POINT('',#8244) ;
#2304 = VERTEX_POINT('',#8245) ;
#2305 = VERTEX_POINT('',#8250) ;
#2306 = VERTEX_POINT('',#8251) ;
#2307 = VERTEX_POINT('',#8259) ;
#2308 = VERTEX_POINT('',#8261) ;
#2309 = VERTEX_POINT('',#8265) ;
#2310 = VERTEX_POINT('',#8269) ;
#2311 = VERTEX_POINT('',#8270) ;
#2312 = VERTEX_POINT('',#8272) ;
#2313 = VERTEX_POINT('',#8274) ;
#2314 = VERTEX_POINT('',#8276) ;
#2315 = VERTEX_POINT('',#8278) ;
#2316 = VERTEX_POINT('',#8281) ;
#2317 = VERTEX_POINT('',#8284) ;
#2318 = VERTEX_POINT('',#8286) ;
#2319 = VERTEX_POINT('',#8290) ;
#2320 = VERTEX_POINT('',#8294) ;
#2321 = VERTEX_POINT('',#8296) ;
#2322 = VERTEX_POINT('',#8298) ;
#2323 = VERTEX_POINT('',#8302) ;
#2324 = VERTEX_POINT('',#8303) ;
#2325 = VERTEX_POINT('',#8305) ;
#2326 = VERTEX_POINT('',#8307) ;
#2327 = VERTEX_POINT('',#8309) ;
#2328 = VERTEX_POINT('',#8311) ;
#2329 = VERTEX_POINT('',#8314) ;
#2330 = VERTEX_POINT('',#8315) ;
#2331 = VERTEX_POINT('',#8317) ;
#2332 = VERTEX_POINT('',#8319) ;
#2333 = VERTEX_POINT('',#8323) ;
#2334 = VERTEX_POINT('',#8327) ;
#2335 = VERTEX_POINT('',#8329) ;
#2336 = VERTEX_POINT('',#8333) ;
#2337 = VERTEX_POINT('',#8337) ;
#2338 = VERTEX_POINT('',#8343) ;
#2339 = VERTEX_POINT('',#8345) ;
#2340 = VERTEX_POINT('',#8349) ;
#2341 = VERTEX_POINT('',#8377) ;
#2342 = VERTEX_POINT('',#8381) ;
#2343 = VERTEX_POINT('',#8382) ;
#2344 = VERTEX_POINT('',#8387) ;
#2345 = VERTEX_POINT('',#8389) ;
#2346 = VERTEX_POINT('',#8396) ;
#2347 = VERTEX_POINT('',#8397) ;
#2348 = VERTEX_POINT('',#8440) ;
#2349 = VERTEX_POINT('',#8469) ;
#2350 = VERTEX_POINT('',#8484) ;
#2351 = VERTEX_POINT('',#8518) ;
#2352 = VERTEX_POINT('',#8523) ;
#2353 = VERTEX_POINT('',#8525) ;
#2354 = VERTEX_POINT('',#8530) ;
#2355 = VERTEX_POINT('',#8586) ;
#2356 = VERTEX_POINT('',#8587) ;
#2357 = VERTEX_POINT('',#8592) ;
#2358 = VERTEX_POINT('',#8594) ;
#2359 = VERTEX_POINT('',#8631) ;
#2360 = VERTEX_POINT('',#8632) ;
#2361 = VERTEX_POINT('',#8665) ;
#2362 = VERTEX_POINT('',#8692) ;
#2363 = VERTEX_POINT('',#8702) ;
#2364 = VERTEX_POINT('',#8719) ;
#2365 = VERTEX_POINT('',#8723) ;
#2366 = VERTEX_POINT('',#8727) ;
#2367 = VERTEX_POINT('',#8729) ;
#2368 = VERTEX_POINT('',#8733) ;
#2369 = VERTEX_POINT('',#8734) ;
#2370 = VERTEX_POINT('',#8739) ;
#2371 = VERTEX_POINT('',#8740) ;
#2372 = VERTEX_POINT('',#8769) ;
#2373 = VERTEX_POINT('',#8770) ;
#2374 = VERTEX_POINT('',#8798) ;
#2375 = VERTEX_POINT('',#8800) ;
#2376 = VERTEX_POINT('',#8802) ;
#2377 = VERTEX_POINT('',#8804) ;
#2378 = VERTEX_POINT('',#8812) ;
#2379 = VERTEX_POINT('',#8818) ;
#2380 = VERTEX_POINT('',#8820) ;
#2381 = VERTEX_POINT('',#8822) ;
#2382 = VERTEX_POINT('',#8824) ;
#2383 = VERTEX_POINT('',#8831) ;
#2384 = VERTEX_POINT('',#8832) ;
#2385 = VERTEX_POINT('',#8904) ;
#2386 = VERTEX_POINT('',#8906) ;
#2387 = VERTEX_POINT('',#8933) ;
#2388 = VERTEX_POINT('',#8937) ;
#2389 = VERTEX_POINT('',#8941) ;
#2390 = VERTEX_POINT('',#8945) ;
#2391 = VERTEX_POINT('',#9042) ;
#2392 = VERTEX_POINT('',#9048) ;
#2393 = VERTEX_POINT('',#9054) ;
#2394 = VERTEX_POINT('',#9056) ;
#2395 = VERTEX_POINT('',#9060) ;
#2396 = VERTEX_POINT('',#9064) ;
#2397 = VERTEX_POINT('',#9068) ;
#2398 = VERTEX_POINT('',#9072) ;
#2399 = VERTEX_POINT('',#9076) ;
#2400 = VERTEX_POINT('',#9080) ;
#2401 = VERTEX_POINT('',#9084) ;
#2402 = VERTEX_POINT('',#9088) ;
#2403 = VERTEX_POINT('',#9096) ;
#2404 = VERTEX_POINT('',#9097) ;
#2405 = VERTEX_POINT('',#9108) ;
#2406 = VERTEX_POINT('',#9110) ;
#2407 = VERTEX_POINT('',#9112) ;
#2408 = VERTEX_POINT('',#9116) ;
#2409 = VERTEX_POINT('',#9117) ;
#2410 = VERTEX_POINT('',#9127) ;
#2411 = VERTEX_POINT('',#9129) ;
#2412 = VERTEX_POINT('',#9131) ;
#2413 = VERTEX_POINT('',#9134) ;
#2414 = VERTEX_POINT('',#9137) ;
#2415 = VERTEX_POINT('',#9138) ;
#2416 = VERTEX_POINT('',#9140) ;
#2417 = VERTEX_POINT('',#9142) ;
#2418 = VERTEX_POINT('',#9151) ;
#2419 = VERTEX_POINT('',#9152) ;
#2420 = VERTEX_POINT('',#9155) ;
#2421 = VERTEX_POINT('',#9168) ;
#2422 = VERTEX_POINT('',#9170) ;
#2423 = VERTEX_POINT('',#9172) ;
#2424 = VERTEX_POINT('',#9175) ;
#2425 = VERTEX_POINT('',#9178) ;
#2426 = VERTEX_POINT('',#9179) ;
#2427 = VERTEX_POINT('',#9181) ;
#2428 = VERTEX_POINT('',#9183) ;
#2429 = VERTEX_POINT('',#9187) ;
#2430 = VERTEX_POINT('',#9188) ;
#2431 = VERTEX_POINT('',#9193) ;
#2432 = VERTEX_POINT('',#9194) ;
#2433 = VERTEX_POINT('',#9202) ;
#2434 = VERTEX_POINT('',#9204) ;
#2435 = VERTEX_POINT('',#9208) ;
#2436 = VERTEX_POINT('',#9212) ;
#2437 = VERTEX_POINT('',#9214) ;
#2438 = VERTEX_POINT('',#9216) ;
#2439 = VERTEX_POINT('',#9218) ;
#2440 = VERTEX_POINT('',#9220) ;
#2441 = VERTEX_POINT('',#9222) ;
#2442 = VERTEX_POINT('',#9224) ;
#2443 = VERTEX_POINT('',#9226) ;
#2444 = VERTEX_POINT('',#9230) ;
#2445 = VERTEX_POINT('',#9231) ;
#2446 = VERTEX_POINT('',#9233) ;
#2447 = VERTEX_POINT('',#9235) ;
#2448 = VERTEX_POINT('',#9239) ;
#2449 = VERTEX_POINT('',#9241) ;
#2450 = VERTEX_POINT('',#9245) ;
#2451 = VERTEX_POINT('',#9249) ;
#2452 = VERTEX_POINT('',#9255) ;
#2453 = VERTEX_POINT('',#9257) ;
#2454 = VERTEX_POINT('',#9261) ;
#2455 = VERTEX_POINT('',#9269) ;
#2456 = VERTEX_POINT('',#9270) ;
#2457 = VERTEX_POINT('',#9313) ;
#2458 = VERTEX_POINT('',#9317) ;
#2459 = VERTEX_POINT('',#9323) ;
#2460 = VERTEX_POINT('',#9324) ;
#2461 = VERTEX_POINT('',#9342) ;
#2462 = VERTEX_POINT('',#9346) ;
#2463 = VERTEX_POINT('',#9352) ;
#2464 = VERTEX_POINT('',#9354) ;
#2465 = VERTEX_POINT('',#9356) ;
#2466 = VERTEX_POINT('',#9360) ;
#2467 = VERTEX_POINT('',#9364) ;
#2468 = VERTEX_POINT('',#9368) ;
#2469 = VERTEX_POINT('',#9372) ;
#2470 = VERTEX_POINT('',#9376) ;
#2471 = VERTEX_POINT('',#9380) ;
#2472 = VERTEX_POINT('',#9384) ;
#2473 = VERTEX_POINT('',#9388) ;
#2474 = VERTEX_POINT('',#9390) ;
#2475 = VERTEX_POINT('',#9394) ;
#2476 = VERTEX_POINT('',#9398) ;
#2477 = VERTEX_POINT('',#9402) ;
#2478 = VERTEX_POINT('',#9404) ;
#2479 = VERTEX_POINT('',#9406) ;
#2480 = VERTEX_POINT('',#9408) ;
#2481 = VERTEX_POINT('',#9410) ;
#2482 = VERTEX_POINT('',#9414) ;
#2483 = VERTEX_POINT('',#9415) ;
#2484 = VERTEX_POINT('',#9420) ;
#2485 = VERTEX_POINT('',#9424) ;
#2486 = VERTEX_POINT('',#9428) ;
#2487 = VERTEX_POINT('',#9435) ;
#2488 = VERTEX_POINT('',#9438) ;
#2489 = VERTEX_POINT('',#9452) ;
#2490 = VERTEX_POINT('',#9453) ;
#2491 = VERTEX_POINT('',#9455) ;
#2492 = VERTEX_POINT('',#9468) ;
#2493 = VERTEX_POINT('',#9491) ;
#2494 = VERTEX_POINT('',#9493) ;
#2495 = VERTEX_POINT('',#9508) ;
#2496 = VERTEX_POINT('',#9510) ;
#2497 = VERTEX_POINT('',#9525) ;
#2498 = VERTEX_POINT('',#9527) ;
#2499 = VERTEX_POINT('',#9542) ;
#2500 = VERTEX_POINT('',#9544) ;
#2501 = VERTEX_POINT('',#9559) ;
#2502 = VERTEX_POINT('',#9560) ;
#2503 = VERTEX_POINT('',#9586) ;
#2504 = VERTEX_POINT('',#9588) ;
#2505 = VERTEX_POINT('',#9603) ;
#2506 = VERTEX_POINT('',#9605) ;
#2507 = VERTEX_POINT('',#9620) ;
#2508 = VERTEX_POINT('',#9622) ;
#2509 = VERTEX_POINT('',#9637) ;
#2510 = VERTEX_POINT('',#9639) ;
#2511 = VERTEX_POINT('',#9667) ;
#2512 = VERTEX_POINT('',#9669) ;
#2513 = VERTEX_POINT('',#9684) ;
#2514 = VERTEX_POINT('',#9685) ;
#2515 = VERTEX_POINT('',#9711) ;
#2516 = VERTEX_POINT('',#9713) ;
#2517 = VERTEX_POINT('',#9732) ;
#2518 = VERTEX_POINT('',#9733) ;
#2519 = VERTEX_POINT('',#9735) ;
#2520 = VERTEX_POINT('',#9761) ;
#2521 = VERTEX_POINT('',#9765) ;
#2522 = VERTEX_POINT('',#9767) ;
#2523 = VERTEX_POINT('',#9782) ;
#2524 = VERTEX_POINT('',#9784) ;
#2525 = VERTEX_POINT('',#9812) ;
#2526 = VERTEX_POINT('',#9814) ;
#2527 = VERTEX_POINT('',#9829) ;
#2528 = VERTEX_POINT('',#9830) ;
#2529 = VERTEX_POINT('',#9856) ;
#2530 = VERTEX_POINT('',#9858) ;
#2531 = VERTEX_POINT('',#9868) ;
#2532 = VERTEX_POINT('',#9870) ;
#2533 = VERTEX_POINT('',#9885) ;
#2534 = VERTEX_POINT('',#9886) ;
#2535 = VERTEX_POINT('',#9915) ;
#2536 = VERTEX_POINT('',#9917) ;
#2537 = VERTEX_POINT('',#9937) ;
#2538 = VERTEX_POINT('',#9939) ;
#2539 = VERTEX_POINT('',#9946) ;
#2540 = VERTEX_POINT('',#9948) ;
#2541 = VERTEX_POINT('',#9965) ;
#2542 = VERTEX_POINT('',#9967) ;
#2543 = VERTEX_POINT('',#9984) ;
#2544 = VERTEX_POINT('',#9986) ;
#2545 = VERTEX_POINT('',#10003) ;
#2546 = VERTEX_POINT('',#10005) ;
#2547 = VERTEX_POINT('',#10023) ;
#2548 = VERTEX_POINT('',#10025) ;
#2549 = VERTEX_POINT('',#10029) ;
#2550 = VERTEX_POINT('',#10033) ;
#2551 = VERTEX_POINT('',#10037) ;
#2552 = VERTEX_POINT('',#10041) ;
#2553 = VERTEX_POINT('',#10045) ;
#2554 = VERTEX_POINT('',#10049) ;
#2555 = VERTEX_POINT('',#10053) ;
#2556 = VERTEX_POINT('',#10057) ;
#2557 = VERTEX_POINT('',#10061) ;
#2558 = VERTEX_POINT('',#10065) ;
#2559 = VERTEX_POINT('',#10069) ;
#2560 = VERTEX_POINT('',#10073) ;
#2561 = VERTEX_POINT('',#10077) ;
#2562 = VERTEX_POINT('',#10081) ;
#2563 = VERTEX_POINT('',#10085) ;
#2564 = VERTEX_POINT('',#10086) ;
#2565 = VERTEX_POINT('',#10088) ;
#2566 = VERTEX_POINT('',#10090) ;
#2567 = VERTEX_POINT('',#10093) ;
#2568 = VERTEX_POINT('',#10096) ;
#2569 = VERTEX_POINT('',#10097) ;
#2570 = VERTEX_POINT('',#10124) ;
#2571 = VERTEX_POINT('',#10126) ;
#2572 = VERTEX_POINT('',#10143) ;
#2573 = VERTEX_POINT('',#10145) ;
#2574 = VERTEX_POINT('',#10160) ;
#2575 = VERTEX_POINT('',#10162) ;
#2576 = VERTEX_POINT('',#10177) ;
#2577 = VERTEX_POINT('',#10179) ;
#2578 = VERTEX_POINT('',#10194) ;
#2579 = VERTEX_POINT('',#10220) ;
#2580 = VERTEX_POINT('',#10235) ;
#2581 = VERTEX_POINT('',#10236) ;
#2582 = VERTEX_POINT('',#10262) ;
#2583 = VERTEX_POINT('',#10264) ;
#2584 = VERTEX_POINT('',#10268) ;
#2585 = VERTEX_POINT('',#10270) ;
#2586 = VERTEX_POINT('',#10287) ;
#2587 = VERTEX_POINT('',#10315) ;
#2588 = VERTEX_POINT('',#10317) ;
#2589 = VERTEX_POINT('',#10332) ;
#2590 = VERTEX_POINT('',#10334) ;
#2591 = VERTEX_POINT('',#10338) ;
#2592 = VERTEX_POINT('',#10364) ;
#2593 = VERTEX_POINT('',#10368) ;
#2594 = VERTEX_POINT('',#10369) ;
#2595 = VERTEX_POINT('',#10398) ;
#2596 = VERTEX_POINT('',#10413) ;
#2597 = VERTEX_POINT('',#10414) ;
#2598 = VERTEX_POINT('',#10443) ;
#2599 = VERTEX_POINT('',#10461) ;
#2600 = VERTEX_POINT('',#10478) ;
#2601 = VERTEX_POINT('',#10479) ;
#2602 = VERTEX_POINT('',#10508) ;
#2603 = VERTEX_POINT('',#10523) ;
#2604 = VERTEX_POINT('',#10525) ;
#2605 = VERTEX_POINT('',#10543) ;
#2606 = VERTEX_POINT('',#10558) ;
#2607 = VERTEX_POINT('',#10573) ;
#2608 = VERTEX_POINT('',#10588) ;
#2609 = VERTEX_POINT('',#10611) ;
#2610 = VERTEX_POINT('',#10655) ;
#2611 = VERTEX_POINT('',#10656) ;
#2612 = VERTEX_POINT('',#10658) ;
#2613 = VERTEX_POINT('',#10660) ;
#2614 = VERTEX_POINT('',#10663) ;
#2615 = VERTEX_POINT('',#10666) ;
#2616 = VERTEX_POINT('',#10679) ;
#2617 = VERTEX_POINT('',#10694) ;
#2618 = VERTEX_POINT('',#10709) ;
#2619 = VERTEX_POINT('',#10726) ;
#2620 = VERTEX_POINT('',#10728) ;
#2621 = VERTEX_POINT('',#10732) ;
#2622 = VERTEX_POINT('',#10736) ;
#2623 = VERTEX_POINT('',#10797) ;
#2624 = VERTEX_POINT('',#10800) ;
#2625 = VERTEX_POINT('',#10804) ;
#2626 = VERTEX_POINT('',#10808) ;
#2627 = VERTEX_POINT('',#10814) ;
#2628 = VERTEX_POINT('',#10817) ;
#2629 = VERTEX_POINT('',#10821) ;
#2630 = VERTEX_POINT('',#10824) ;
#2631 = VERTEX_POINT('',#10828) ;
#2632 = VERTEX_POINT('',#10832) ;
#2633 = VERTEX_POINT('',#10836) ;
#2634 = VERTEX_POINT('',#10839) ;
#2635 = VERTEX_POINT('',#10845) ;
#2636 = VERTEX_POINT('',#10848) ;
#2637 = VERTEX_POINT('',#10852) ;
#2638 = VERTEX_POINT('',#10856) ;
#2639 = VERTEX_POINT('',#10862) ;
#2640 = VERTEX_POINT('',#10864) ;
#2641 = VERTEX_POINT('',#10868) ;
#2642 = VERTEX_POINT('',#10869) ;
#2643 = VERTEX_POINT('',#10871) ;
#2644 = VERTEX_POINT('',#10873) ;
#2645 = VERTEX_POINT('',#10877) ;
#2646 = VERTEX_POINT('',#10879) ;
#2647 = VERTEX_POINT('',#10883) ;
#2648 = VERTEX_POINT('',#10885) ;
#2649 = VERTEX_POINT('',#10889) ;
#2650 = VERTEX_POINT('',#10891) ;
#2651 = VERTEX_POINT('',#10895) ;
#2652 = VERTEX_POINT('',#10897) ;
#2653 = VERTEX_POINT('',#10901) ;
#2654 = VERTEX_POINT('',#10903) ;
#2655 = VERTEX_POINT('',#10907) ;
#2656 = VERTEX_POINT('',#10909) ;
#2657 = VERTEX_POINT('',#10913) ;
#2658 = VERTEX_POINT('',#10915) ;
#2659 = VERTEX_POINT('',#10925) ;
#2660 = VERTEX_POINT('',#10926) ;
#2661 = VERTEX_POINT('',#10928) ;
#2662 = VERTEX_POINT('',#10930) ;
#2663 = VERTEX_POINT('',#10934) ;
#2664 = VERTEX_POINT('',#10936) ;
#2665 = VERTEX_POINT('',#10940) ;
#2666 = VERTEX_POINT('',#10942) ;
#2667 = VERTEX_POINT('',#10946) ;
#2668 = VERTEX_POINT('',#10948) ;
#2669 = VERTEX_POINT('',#10952) ;
#2670 = VERTEX_POINT('',#10954) ;
#2671 = VERTEX_POINT('',#10962) ;
#2672 = VERTEX_POINT('',#10965) ;
#2673 = VERTEX_POINT('',#10969) ;
#2674 = VERTEX_POINT('',#10973) ;
#2675 = VERTEX_POINT('',#10977) ;
#2676 = VERTEX_POINT('',#10981) ;
#2677 = VERTEX_POINT('',#10987) ;
#2678 = VERTEX_POINT('',#10989) ;
#2679 = VERTEX_POINT('',#10991) ;
#2680 = VERTEX_POINT('',#11006) ;
#2681 = VERTEX_POINT('',#11035) ;
#2682 = VERTEX_POINT('',#11077) ;
#2683 = VERTEX_POINT('',#11080) ;
#2684 = VERTEX_POINT('',#11082) ;
#2685 = VERTEX_POINT('',#11087) ;
#2686 = VERTEX_POINT('',#11089) ;
#2687 = VERTEX_POINT('',#11091) ;
#2688 = VERTEX_POINT('',#11122) ;
#2689 = VERTEX_POINT('',#11124) ;
#2690 = VERTEX_POINT('',#11154) ;
#2691 = VERTEX_POINT('',#11157) ;
#2692 = VERTEX_POINT('',#11164) ;
#2693 = VERTEX_POINT('',#11166) ;
#2694 = VERTEX_POINT('',#11170) ;
#2695 = VERTEX_POINT('',#11173) ;
#2696 = VERTEX_POINT('',#11179) ;
#2697 = VERTEX_POINT('',#11181) ;
#2698 = VERTEX_POINT('',#11185) ;
#2699 = VERTEX_POINT('',#11188) ;
#2700 = VERTEX_POINT('',#11194) ;
#2701 = VERTEX_POINT('',#11196) ;
#2702 = VERTEX_POINT('',#11200) ;
#2703 = VERTEX_POINT('',#11203) ;
#2704 = VERTEX_POINT('',#11209) ;
#2705 = VERTEX_POINT('',#11210) ;
#2706 = VERTEX_POINT('',#11212) ;
#2707 = VERTEX_POINT('',#11214) ;
#2708 = VERTEX_POINT('',#11218) ;
#2709 = VERTEX_POINT('',#11220) ;
#2710 = VERTEX_POINT('',#11224) ;
#2711 = VERTEX_POINT('',#11226) ;
#2712 = VERTEX_POINT('',#11230) ;
#2713 = VERTEX_POINT('',#11232) ;
#2714 = VERTEX_POINT('',#11236) ;
#2715 = VERTEX_POINT('',#11238) ;
#2716 = VERTEX_POINT('',#11242) ;
#2717 = VERTEX_POINT('',#11244) ;
#2718 = VERTEX_POINT('',#11248) ;
#2719 = VERTEX_POINT('',#11250) ;
#2720 = VERTEX_POINT('',#11260) ;
#2721 = VERTEX_POINT('',#11262) ;
#2722 = VERTEX_POINT('',#11266) ;
#2723 = VERTEX_POINT('',#11267) ;
#2724 = VERTEX_POINT('',#11269) ;
#2725 = VERTEX_POINT('',#11271) ;
#2726 = VERTEX_POINT('',#11275) ;
#2727 = VERTEX_POINT('',#11277) ;
#2728 = VERTEX_POINT('',#11281) ;
#2729 = VERTEX_POINT('',#11283) ;
#2730 = VERTEX_POINT('',#11287) ;
#2731 = VERTEX_POINT('',#11289) ;
#2732 = VERTEX_POINT('',#11293) ;
#2733 = VERTEX_POINT('',#11295) ;
#2734 = VERTEX_POINT('',#11299) ;
#2735 = VERTEX_POINT('',#11301) ;
#2736 = VERTEX_POINT('',#11305) ;
#2737 = VERTEX_POINT('',#11307) ;
#2738 = VERTEX_POINT('',#11311) ;
#2739 = VERTEX_POINT('',#11313) ;
#2740 = VERTEX_POINT('',#11317) ;
#2741 = VERTEX_POINT('',#11319) ;
#2742 = VERTEX_POINT('',#11329) ;
#2743 = VERTEX_POINT('',#11331) ;
#2744 = VERTEX_POINT('',#11335) ;
#2745 = VERTEX_POINT('',#11338) ;
#2746 = EDGE_CURVE('',#2269,#2269,#1987,.T.) ;
#2747 = EDGE_CURVE('',#2269,#2270,#1221,.T.) ;
#2748 = EDGE_CURVE('',#2270,#2270,#1988,.T.) ;
#2749 = EDGE_CURVE('',#2271,#2271,#1989,.T.) ;
#2750 = EDGE_CURVE('',#2271,#2272,#1222,.T.) ;
#2751 = EDGE_CURVE('',#2272,#2272,#1990,.T.) ;
#2752 = EDGE_CURVE('',#2273,#2273,#1991,.T.) ;
#2753 = EDGE_CURVE('',#2273,#2274,#1223,.T.) ;
#2754 = EDGE_CURVE('',#2274,#2274,#1992,.T.) ;
#2755 = EDGE_CURVE('',#2275,#2276,#378,.T.) ;
#2756 = EDGE_CURVE('',#2277,#2275,#1224,.T.) ;
#2757 = EDGE_CURVE('',#2277,#2278,#1225,.T.) ;
#2758 = EDGE_CURVE('',#2278,#2279,#1226,.T.) ;
#2759 = EDGE_CURVE('',#2280,#2279,#379,.T.) ;
#2760 = EDGE_CURVE('',#2276,#2280,#1227,.T.) ;
#2761 = EDGE_CURVE('',#2279,#2281,#1228,.T.) ;
#2762 = EDGE_CURVE('',#2282,#2278,#1229,.T.) ;
#2763 = EDGE_CURVE('',#2283,#2282,#1230,.T.) ;
#2764 = EDGE_CURVE('',#2284,#2283,#1231,.T.) ;
#2765 = EDGE_CURVE('',#2285,#2284,#1232,.T.) ;
#2766 = EDGE_CURVE('',#2286,#2285,#1233,.T.) ;
#2767 = EDGE_CURVE('',#2281,#2286,#1234,.T.) ;
#2768 = EDGE_CURVE('',#2287,#2277,#1235,.T.) ;
#2769 = EDGE_CURVE('',#2287,#2282,#1236,.T.) ;
#2770 = EDGE_CURVE('',#2288,#2287,#1237,.T.) ;
#2771 = EDGE_CURVE('',#2288,#2283,#1238,.T.) ;
#2772 = EDGE_CURVE('',#2289,#2288,#1239,.T.) ;
#2773 = EDGE_CURVE('',#2289,#2284,#1240,.T.) ;
#2774 = EDGE_CURVE('',#2285,#2290,#1241,.T.) ;
#2775 = EDGE_CURVE('',#2290,#2289,#1242,.T.) ;
#2776 = EDGE_CURVE('',#2291,#2275,#1243,.T.) ;
#2777 = EDGE_CURVE('',#2292,#2291,#1244,.T.) ;
#2778 = EDGE_CURVE('',#2290,#2292,#1245,.T.) ;
#2779 = EDGE_CURVE('',#2293,#2280,#1246,.T.) ;
#2780 = EDGE_CURVE('',#2294,#2293,#1247,.T.) ;
#2781 = EDGE_CURVE('',#2276,#2294,#1248,.T.) ;
#2782 = EDGE_CURVE('',#2281,#2295,#380,.T.) ;
#2783 = EDGE_CURVE('',#2296,#2295,#381,.T.) ;
#2784 = EDGE_CURVE('',#2296,#2297,#1249,.T.) ;
#2785 = EDGE_CURVE('',#2297,#2293,#382,.T.) ;
#2786 = EDGE_CURVE('',#2286,#2298,#1250,.T.) ;
#2787 = EDGE_CURVE('',#2295,#2298,#238,.T.) ;
#2788 = EDGE_CURVE('',#2299,#2300,#1993,.T.) ;
#2789 = EDGE_CURVE('',#2300,#2301,#1994,.T.) ;
#2790 = EDGE_CURVE('',#2301,#2302,#1995,.T.) ;
#2791 = EDGE_CURVE('',#2302,#2299,#1996,.T.) ;
#2792 = EDGE_CURVE('',#2303,#2304,#1997,.T.) ;
#2793 = EDGE_CURVE('',#2304,#2302,#1251,.T.) ;
#2794 = EDGE_CURVE('',#2301,#2303,#1252,.T.) ;
#2795 = EDGE_CURVE('',#2305,#2306,#1998,.T.) ;
#2796 = EDGE_CURVE('',#2306,#2304,#1999,.T.) ;
#2797 = EDGE_CURVE('',#2303,#2305,#2000,.T.) ;
#2798 = EDGE_CURVE('',#2299,#2306,#1253,.T.) ;
#2799 = EDGE_CURVE('',#2305,#2300,#1254,.T.) ;
#2800 = EDGE_CURVE('',#2307,#2301,#1255,.T.) ;
#2801 = EDGE_CURVE('',#2307,#2308,#1256,.T.) ;
#2802 = EDGE_CURVE('',#2308,#2303,#1257,.T.) ;
#2803 = EDGE_CURVE('',#2309,#2300,#1258,.T.) ;
#2804 = EDGE_CURVE('',#2309,#2307,#2001,.T.) ;
#2805 = EDGE_CURVE('',#2310,#2311,#2002,.T.) ;
#2806 = EDGE_CURVE('',#2312,#2310,#1259,.T.) ;
#2807 = EDGE_CURVE('',#2313,#2312,#2003,.T.) ;
#2808 = EDGE_CURVE('',#2314,#2313,#1260,.T.) ;
#2809 = EDGE_CURVE('',#2315,#2314,#1261,.T.) ;
#2810 = EDGE_CURVE('',#2311,#2315,#1262,.T.) ;
#2811 = EDGE_CURVE('',#2316,#2316,#2004,.T.) ;
#2812 = EDGE_CURVE('',#2316,#2317,#2005,.T.) ;
#2813 = EDGE_CURVE('',#2317,#2318,#2006,.T.) ;
#2814 = EDGE_CURVE('',#2318,#2317,#2007,.T.) ;
#2815 = EDGE_CURVE('',#2318,#2319,#1263,.T.) ;
#2816 = EDGE_CURVE('',#2319,#2319,#2008,.T.) ;
#2817 = EDGE_CURVE('',#2320,#2320,#2009,.T.) ;
#2818 = EDGE_CURVE('',#2320,#2321,#2010,.T.) ;
#2819 = EDGE_CURVE('',#2321,#2322,#2011,.T.) ;
#2820 = EDGE_CURVE('',#2322,#2321,#2012,.T.) ;
#2821 = EDGE_CURVE('',#2323,#2324,#1264,.T.) ;
#2822 = EDGE_CURVE('',#2325,#2323,#1265,.T.) ;
#2823 = EDGE_CURVE('',#2326,#2325,#2013,.T.) ;
#2824 = EDGE_CURVE('',#2327,#2326,#1266,.T.) ;
#2825 = EDGE_CURVE('',#2328,#2327,#2014,.T.) ;
#2826 = EDGE_CURVE('',#2324,#2328,#1267,.T.) ;
#2827 = EDGE_CURVE('',#2329,#2330,#2015,.T.) ;
#2828 = EDGE_CURVE('',#2331,#2329,#1268,.T.) ;
#2829 = EDGE_CURVE('',#2332,#2331,#2016,.T.) ;
#2830 = EDGE_CURVE('',#2330,#2332,#1269,.T.) ;
#2831 = EDGE_CURVE('',#2322,#2333,#1270,.T.) ;
#2832 = EDGE_CURVE('',#2333,#2333,#2017,.T.) ;
#2833 = EDGE_CURVE('',#2330,#2334,#2018,.T.) ;
#2834 = EDGE_CURVE('',#2334,#2335,#2019,.T.) ;
#2835 = EDGE_CURVE('',#2335,#2329,#2020,.T.) ;
#2836 = EDGE_CURVE('',#2336,#2331,#2021,.T.) ;
#2837 = EDGE_CURVE('',#2335,#2336,#1271,.T.) ;
#2838 = EDGE_CURVE('',#2337,#2332,#2022,.T.) ;
#2839 = EDGE_CURVE('',#2336,#2337,#2023,.T.) ;
#2840 = EDGE_CURVE('',#2337,#2334,#1272,.T.) ;
#2841 = EDGE_CURVE('',#2338,#2335,#1273,.T.) ;
#2842 = EDGE_CURVE('',#2338,#2339,#1274,.T.) ;
#2843 = EDGE_CURVE('',#2339,#2336,#1275,.T.) ;
#2844 = EDGE_CURVE('',#2340,#2334,#1276,.T.) ;
#2845 = EDGE_CURVE('',#2340,#2338,#2024,.T.) ;
#2846 = EDGE_CURVE('',#2298,#2341,#383,.T.) ;
#2847 = EDGE_CURVE('',#2341,#2296,#2025,.T.) ;
#2848 = EDGE_CURVE('',#2342,#2343,#2026,.T.) ;
#2849 = EDGE_CURVE('',#2343,#2296,#1277,.T.) ;
#2850 = EDGE_CURVE('',#2341,#2342,#1278,.T.) ;
#2851 = EDGE_CURVE('',#2324,#2344,#2027,.T.) ;
#2852 = EDGE_CURVE('',#2344,#2345,#1279,.T.) ;
#2853 = EDGE_CURVE('',#2345,#2323,#2028,.T.) ;
#2854 = EDGE_CURVE('',#2324,#2343,#2029,.T.) ;
#2855 = EDGE_CURVE('',#2342,#2344,#2030,.T.) ;
#2856 = EDGE_CURVE('',#2346,#2347,#2031,.T.) ;
#2857 = EDGE_CURVE('',#2347,#2326,#239,.T.) ;
#2858 = EDGE_CURVE('',#2325,#2346,#240,.T.) ;
#2859 = EDGE_CURVE('',#2348,#2313,#241,.T.) ;
#2860 = EDGE_CURVE('',#2312,#2349,#242,.T.) ;
#2861 = EDGE_CURVE('',#2349,#2348,#2032,.T.) ;
#2862 = EDGE_CURVE('',#2310,#2350,#243,.T.) ;
#2863 = EDGE_CURVE('',#2350,#2349,#1280,.T.) ;
#2864 = EDGE_CURVE('',#2351,#2328,#244,.T.) ;
#2865 = EDGE_CURVE('',#2328,#2352,#2033,.T.) ;
#2866 = EDGE_CURVE('',#2352,#2353,#245,.T.) ;
#2867 = EDGE_CURVE('',#2353,#2354,#246,.T.) ;
#2868 = EDGE_CURVE('',#2354,#2351,#247,.T.) ;
#2869 = EDGE_CURVE('',#2355,#2356,#248,.T.) ;
#2870 = EDGE_CURVE('',#2356,#2357,#2034,.T.) ;
#2871 = EDGE_CURVE('',#2357,#2358,#249,.T.) ;
#2872 = EDGE_CURVE('',#2358,#2355,#250,.T.) ;
#2873 = EDGE_CURVE('',#2359,#2360,#2035,.T.) ;
#2874 = EDGE_CURVE('',#2360,#2357,#2036,.T.) ;
#2875 = EDGE_CURVE('',#2356,#2359,#2037,.T.) ;
#2876 = EDGE_CURVE('',#2353,#2360,#251,.T.) ;
#2877 = EDGE_CURVE('',#2359,#2354,#252,.T.) ;
#2878 = EDGE_CURVE('',#2311,#2361,#2038,.T.) ;
#2879 = EDGE_CURVE('',#2361,#2350,#2039,.T.) ;
#2880 = EDGE_CURVE('',#2358,#2361,#253,.T.) ;
#2881 = EDGE_CURVE('',#2311,#2362,#254,.T.) ;
#2882 = EDGE_CURVE('',#2362,#2355,#255,.T.) ;
#2883 = EDGE_CURVE('',#2363,#2352,#2040,.T.) ;
#2884 = EDGE_CURVE('',#2327,#2363,#256,.T.) ;
#2885 = EDGE_CURVE('',#2347,#2363,#1281,.T.) ;
#2886 = EDGE_CURVE('',#2348,#2364,#1282,.T.) ;
#2887 = EDGE_CURVE('',#2364,#2314,#2041,.T.) ;
#2888 = EDGE_CURVE('',#2323,#2365,#2042,.T.) ;
#2889 = EDGE_CURVE('',#2365,#2346,#1283,.T.) ;
#2890 = EDGE_CURVE('',#2314,#2366,#2043,.T.) ;
#2891 = EDGE_CURVE('',#2366,#2367,#1284,.T.) ;
#2892 = EDGE_CURVE('',#2367,#2315,#2044,.T.) ;
#2893 = EDGE_CURVE('',#2368,#2369,#2045,.T.) ;
#2894 = EDGE_CURVE('',#2369,#2315,#2046,.T.) ;
#2895 = EDGE_CURVE('',#2367,#2368,#2047,.T.) ;
#2896 = EDGE_CURVE('',#2370,#2371,#2048,.T.) ;
#2897 = EDGE_CURVE('',#2371,#2369,#1285,.T.) ;
#2898 = EDGE_CURVE('',#2368,#2370,#1286,.T.) ;
#2899 = EDGE_CURVE('',#2372,#2373,#257,.T.) ;
#2900 = EDGE_CURVE('',#2373,#2371,#384,.T.) ;
#2901 = EDGE_CURVE('',#2370,#2372,#385,.T.) ;
#2902 = EDGE_CURVE('',#2364,#2366,#2049,.T.) ;
#2903 = EDGE_CURVE('',#2345,#2365,#2050,.T.) ;
#2904 = EDGE_CURVE('',#2374,#2343,#1287,.T.) ;
#2905 = EDGE_CURVE('',#2374,#2375,#1288,.T.) ;
#2906 = EDGE_CURVE('',#2376,#2375,#1289,.T.) ;
#2907 = EDGE_CURVE('',#2377,#2376,#2051,.T.) ;
#2908 = EDGE_CURVE('',#2297,#2377,#1290,.T.) ;
#2909 = EDGE_CURVE('',#2374,#2351,#386,.T.) ;
#2910 = EDGE_CURVE('',#2359,#2356,#1291,.T.) ;
#2911 = EDGE_CURVE('',#2362,#2378,#387,.T.) ;
#2912 = EDGE_CURVE('',#2378,#2374,#1292,.T.) ;
#2913 = EDGE_CURVE('',#2369,#2378,#1293,.T.) ;
#2914 = EDGE_CURVE('',#2379,#2371,#1294,.T.) ;
#2915 = EDGE_CURVE('',#2380,#2379,#1295,.T.) ;
#2916 = EDGE_CURVE('',#2381,#2380,#2052,.T.) ;
#2917 = EDGE_CURVE('',#2382,#2381,#1296,.T.) ;
#2918 = EDGE_CURVE('',#2378,#2382,#1297,.T.) ;
#2919 = EDGE_CURVE('',#2379,#2294,#388,.T.) ;
#2920 = EDGE_CURVE('',#2373,#2291,#389,.T.) ;
#2921 = EDGE_CURVE('',#2383,#2384,#2053,.T.) ;
#2922 = EDGE_CURVE('',#2384,#2377,#258,.T.) ;
#2923 = EDGE_CURVE('',#2376,#2383,#259,.T.) ;
#2924 = EDGE_CURVE('',#2384,#2293,#1298,.T.) ;
#2925 = EDGE_CURVE('',#2375,#2385,#390,.T.) ;
#2926 = EDGE_CURVE('',#2385,#2386,#260,.T.) ;
#2927 = EDGE_CURVE('',#2386,#2383,#1299,.T.) ;
#2928 = EDGE_CURVE('',#2372,#2292,#1300,.T.) ;
#2929 = EDGE_CURVE('',#2387,#2384,#1301,.T.) ;
#2930 = EDGE_CURVE('',#2294,#2387,#1302,.T.) ;
#2931 = EDGE_CURVE('',#2388,#2383,#1303,.T.) ;
#2932 = EDGE_CURVE('',#2387,#2388,#2054,.T.) ;
#2933 = EDGE_CURVE('',#2389,#2386,#1304,.T.) ;
#2934 = EDGE_CURVE('',#2388,#2389,#1305,.T.) ;
#2935 = EDGE_CURVE('',#2390,#2385,#1306,.T.) ;
#2936 = EDGE_CURVE('',#2389,#2390,#261,.T.) ;
#2937 = EDGE_CURVE('',#2390,#2382,#391,.T.) ;
#2938 = EDGE_CURVE('',#2381,#2388,#262,.T.) ;
#2939 = EDGE_CURVE('',#2387,#2380,#263,.T.) ;
#2940 = EDGE_CURVE('',#2391,#2305,#1307,.T.) ;
#2941 = EDGE_CURVE('',#2391,#2309,#1308,.T.) ;
#2942 = EDGE_CURVE('',#2308,#2391,#2055,.T.) ;
#2943 = EDGE_CURVE('',#2392,#2337,#1309,.T.) ;
#2944 = EDGE_CURVE('',#2392,#2340,#1310,.T.) ;
#2945 = EDGE_CURVE('',#2339,#2392,#2056,.T.) ;
#2946 = EDGE_CURVE('',#2393,#2348,#1311,.T.) ;
#2947 = EDGE_CURVE('',#2394,#2393,#1312,.T.) ;
#2948 = EDGE_CURVE('',#2394,#2364,#1313,.T.) ;
#2949 = EDGE_CURVE('',#2395,#2349,#1314,.T.) ;
#2950 = EDGE_CURVE('',#2395,#2393,#2057,.T.) ;
#2951 = EDGE_CURVE('',#2396,#2350,#1315,.T.) ;
#2952 = EDGE_CURVE('',#2395,#2396,#1316,.T.) ;
#2953 = EDGE_CURVE('',#2397,#2363,#1317,.T.) ;
#2954 = EDGE_CURVE('',#2397,#2396,#2058,.T.) ;
#2955 = EDGE_CURVE('',#2398,#2347,#1318,.T.) ;
#2956 = EDGE_CURVE('',#2397,#2398,#1319,.T.) ;
#2957 = EDGE_CURVE('',#2399,#2346,#1320,.T.) ;
#2958 = EDGE_CURVE('',#2399,#2398,#2059,.T.) ;
#2959 = EDGE_CURVE('',#2400,#2365,#1321,.T.) ;
#2960 = EDGE_CURVE('',#2399,#2400,#1322,.T.) ;
#2961 = EDGE_CURVE('',#2401,#2345,#1323,.T.) ;
#2962 = EDGE_CURVE('',#2401,#2400,#2060,.T.) ;
#2963 = EDGE_CURVE('',#2402,#2366,#1324,.T.) ;
#2964 = EDGE_CURVE('',#2401,#2402,#1325,.T.) ;
#2965 = EDGE_CURVE('',#2394,#2402,#2061,.T.) ;
#2966 = EDGE_CURVE('',#2403,#2404,#264,.T.) ;
#2967 = EDGE_CURVE('',#2404,#2405,#1326,.T.) ;
#2968 = EDGE_CURVE('',#2405,#2406,#2062,.T.) ;
#2969 = EDGE_CURVE('',#2406,#2407,#1327,.T.) ;
#2970 = EDGE_CURVE('',#2407,#2403,#392,.T.) ;
#2971 = EDGE_CURVE('',#2408,#2409,#265,.T.) ;
#2972 = EDGE_CURVE('',#2409,#2406,#2063,.T.) ;
#2973 = EDGE_CURVE('',#2405,#2408,#2064,.T.) ;
#2974 = EDGE_CURVE('',#2404,#2410,#2065,.T.) ;
#2975 = EDGE_CURVE('',#2411,#2410,#1328,.T.) ;
#2976 = EDGE_CURVE('',#2412,#2411,#2066,.T.) ;
#2977 = EDGE_CURVE('',#2408,#2412,#1329,.T.) ;
#2978 = EDGE_CURVE('',#2413,#2413,#2067,.T.) ;
#2979 = EDGE_CURVE('',#2414,#2415,#2068,.T.) ;
#2980 = EDGE_CURVE('',#2415,#2416,#2069,.T.) ;
#2981 = EDGE_CURVE('',#2416,#2417,#266,.T.) ;
#2982 = EDGE_CURVE('',#2417,#2414,#2070,.T.) ;
#2983 = EDGE_CURVE('',#2418,#2419,#393,.F.) ;
#2984 = EDGE_CURVE('',#2418,#2415,#1330,.T.) ;
#2985 = EDGE_CURVE('',#2414,#2420,#1331,.T.) ;
#2986 = EDGE_CURVE('',#2419,#2420,#267,.F.) ;
#2987 = EDGE_CURVE('',#2417,#2421,#1332,.T.) ;
#2988 = EDGE_CURVE('',#2421,#2422,#2071,.T.) ;
#2989 = EDGE_CURVE('',#2422,#2423,#1333,.T.) ;
#2990 = EDGE_CURVE('',#2423,#2420,#2072,.T.) ;
#2991 = EDGE_CURVE('',#2424,#2424,#2073,.T.) ;
#2992 = EDGE_CURVE('',#2425,#2426,#2074,.T.) ;
#2993 = EDGE_CURVE('',#2426,#2427,#2075,.T.) ;
#2994 = EDGE_CURVE('',#2427,#2428,#2076,.T.) ;
#2995 = EDGE_CURVE('',#2428,#2425,#2077,.T.) ;
#2996 = EDGE_CURVE('',#2429,#2430,#2078,.T.) ;
#2997 = EDGE_CURVE('',#2430,#2428,#1334,.T.) ;
#2998 = EDGE_CURVE('',#2427,#2429,#1335,.T.) ;
#2999 = EDGE_CURVE('',#2431,#2432,#2079,.T.) ;
#3000 = EDGE_CURVE('',#2432,#2430,#2080,.T.) ;
#3001 = EDGE_CURVE('',#2429,#2431,#2081,.T.) ;
#3002 = EDGE_CURVE('',#2425,#2432,#1336,.T.) ;
#3003 = EDGE_CURVE('',#2431,#2426,#1337,.T.) ;
#3004 = EDGE_CURVE('',#2433,#2427,#1338,.T.) ;
#3005 = EDGE_CURVE('',#2433,#2434,#1339,.T.) ;
#3006 = EDGE_CURVE('',#2434,#2429,#1340,.T.) ;
#3007 = EDGE_CURVE('',#2435,#2426,#1341,.T.) ;
#3008 = EDGE_CURVE('',#2435,#2433,#2082,.T.) ;
#3009 = EDGE_CURVE('',#2436,#2406,#1342,.T.) ;
#3010 = EDGE_CURVE('',#2437,#2436,#2083,.T.) ;
#3011 = EDGE_CURVE('',#2438,#2437,#1343,.T.) ;
#3012 = EDGE_CURVE('',#2439,#2438,#2084,.T.) ;
#3013 = EDGE_CURVE('',#2440,#2439,#2085,.T.) ;
#3014 = EDGE_CURVE('',#2441,#2440,#2086,.T.) ;
#3015 = EDGE_CURVE('',#2442,#2441,#1344,.T.) ;
#3016 = EDGE_CURVE('',#2443,#2442,#2087,.T.) ;
#3017 = EDGE_CURVE('',#2415,#2443,#1345,.T.) ;
#3018 = EDGE_CURVE('',#2407,#2418,#1346,.T.) ;
#3019 = EDGE_CURVE('',#2444,#2445,#2088,.T.) ;
#3020 = EDGE_CURVE('',#2446,#2444,#1347,.T.) ;
#3021 = EDGE_CURVE('',#2447,#2446,#2089,.T.) ;
#3022 = EDGE_CURVE('',#2445,#2447,#1348,.T.) ;
#3023 = EDGE_CURVE('',#2445,#2448,#2090,.T.) ;
#3024 = EDGE_CURVE('',#2448,#2449,#2091,.T.) ;
#3025 = EDGE_CURVE('',#2449,#2444,#2092,.T.) ;
#3026 = EDGE_CURVE('',#2450,#2446,#2093,.T.) ;
#3027 = EDGE_CURVE('',#2449,#2450,#1349,.T.) ;
#3028 = EDGE_CURVE('',#2451,#2447,#2094,.T.) ;
#3029 = EDGE_CURVE('',#2450,#2451,#2095,.T.) ;
#3030 = EDGE_CURVE('',#2451,#2448,#1350,.T.) ;
#3031 = EDGE_CURVE('',#2452,#2449,#1351,.T.) ;
#3032 = EDGE_CURVE('',#2452,#2453,#1352,.T.) ;
#3033 = EDGE_CURVE('',#2453,#2450,#1353,.T.) ;
#3034 = EDGE_CURVE('',#2454,#2448,#1354,.T.) ;
#3035 = EDGE_CURVE('',#2454,#2452,#2096,.T.) ;
#3036 = EDGE_CURVE('',#2419,#2403,#1355,.T.) ;
#3037 = EDGE_CURVE('',#2410,#2423,#1356,.T.) ;
#3038 = EDGE_CURVE('',#2455,#2456,#2097,.T.) ;
#3039 = EDGE_CURVE('',#2456,#2441,#268,.T.) ;
#3040 = EDGE_CURVE('',#2440,#2455,#269,.T.) ;
#3041 = EDGE_CURVE('',#2456,#2457,#1357,.T.) ;
#3042 = EDGE_CURVE('',#2457,#2442,#2098,.T.) ;
#3043 = EDGE_CURVE('',#2458,#2443,#2099,.T.) ;
#3044 = EDGE_CURVE('',#2457,#2458,#2100,.T.) ;
#3045 = EDGE_CURVE('',#2458,#2416,#1358,.T.) ;
#3046 = EDGE_CURVE('',#2459,#2460,#2101,.T.) ;
#3047 = EDGE_CURVE('',#2460,#2439,#2102,.T.) ;
#3048 = EDGE_CURVE('',#2438,#2459,#270,.T.) ;
#3049 = EDGE_CURVE('',#2460,#2455,#2103,.T.) ;
#3050 = EDGE_CURVE('',#2409,#2461,#1359,.T.) ;
#3051 = EDGE_CURVE('',#2461,#2436,#2104,.T.) ;
#3052 = EDGE_CURVE('',#2462,#2437,#2105,.T.) ;
#3053 = EDGE_CURVE('',#2461,#2462,#2106,.T.) ;
#3054 = EDGE_CURVE('',#2462,#2459,#1360,.T.) ;
#3055 = EDGE_CURVE('',#2463,#2458,#1361,.T.) ;
#3056 = EDGE_CURVE('',#2464,#2463,#1362,.T.) ;
#3057 = EDGE_CURVE('',#2464,#2465,#1363,.T.) ;
#3058 = EDGE_CURVE('',#2465,#2421,#1364,.T.) ;
#3059 = EDGE_CURVE('',#2466,#2457,#1365,.T.) ;
#3060 = EDGE_CURVE('',#2466,#2463,#2107,.T.) ;
#3061 = EDGE_CURVE('',#2467,#2456,#1366,.T.) ;
#3062 = EDGE_CURVE('',#2466,#2467,#1367,.T.) ;
#3063 = EDGE_CURVE('',#2468,#2455,#1368,.T.) ;
#3064 = EDGE_CURVE('',#2468,#2467,#2108,.T.) ;
#3065 = EDGE_CURVE('',#2469,#2460,#1369,.T.) ;
#3066 = EDGE_CURVE('',#2469,#2468,#2109,.T.) ;
#3067 = EDGE_CURVE('',#2470,#2459,#1370,.T.) ;
#3068 = EDGE_CURVE('',#2470,#2469,#2110,.T.) ;
#3069 = EDGE_CURVE('',#2471,#2462,#1371,.T.) ;
#3070 = EDGE_CURVE('',#2470,#2471,#1372,.T.) ;
#3071 = EDGE_CURVE('',#2472,#2461,#1373,.T.) ;
#3072 = EDGE_CURVE('',#2472,#2471,#2111,.T.) ;
#3073 = EDGE_CURVE('',#2412,#2473,#1374,.T.) ;
#3074 = EDGE_CURVE('',#2473,#2474,#1375,.T.) ;
#3075 = EDGE_CURVE('',#2472,#2474,#1376,.T.) ;
#3076 = EDGE_CURVE('',#2413,#2475,#1377,.T.) ;
#3077 = EDGE_CURVE('',#2475,#2475,#2112,.T.) ;
#3078 = EDGE_CURVE('',#2476,#2476,#2113,.T.) ;
#3079 = EDGE_CURVE('',#2476,#2424,#1378,.T.) ;
#3080 = EDGE_CURVE('',#2477,#2464,#1379,.T.) ;
#3081 = EDGE_CURVE('',#2478,#2477,#1380,.T.) ;
#3082 = EDGE_CURVE('',#2479,#2478,#1381,.T.) ;
#3083 = EDGE_CURVE('',#2480,#2479,#2114,.T.) ;
#3084 = EDGE_CURVE('',#2481,#2480,#1382,.T.) ;
#3085 = EDGE_CURVE('',#2465,#2481,#2115,.T.) ;
#3086 = EDGE_CURVE('',#2482,#2483,#1383,.T.) ;
#3087 = EDGE_CURVE('',#2482,#2478,#1384,.T.) ;
#3088 = EDGE_CURVE('',#2483,#2477,#1385,.T.) ;
#3089 = EDGE_CURVE('',#2484,#2482,#1386,.T.) ;
#3090 = EDGE_CURVE('',#2484,#2479,#1387,.T.) ;
#3091 = EDGE_CURVE('',#2485,#2484,#2116,.T.) ;
#3092 = EDGE_CURVE('',#2485,#2480,#1388,.T.) ;
#3093 = EDGE_CURVE('',#2481,#2486,#1389,.T.) ;
#3094 = EDGE_CURVE('',#2486,#2485,#1390,.T.) ;
#3095 = EDGE_CURVE('',#2486,#2473,#2117,.T.) ;
#3096 = EDGE_CURVE('',#2474,#2483,#1391,.T.) ;
#3097 = EDGE_CURVE('',#2487,#2454,#1392,.T.) ;
#3098 = EDGE_CURVE('',#2453,#2487,#2118,.T.) ;
#3099 = EDGE_CURVE('',#2488,#2435,#1393,.T.) ;
#3100 = EDGE_CURVE('',#2434,#2488,#2119,.T.) ;
#3101 = EDGE_CURVE('',#2411,#2422,#1394,.T.) ;
#3102 = EDGE_CURVE('',#2487,#2451,#1395,.T.) ;
#3103 = EDGE_CURVE('',#2488,#2431,#1396,.T.) ;
#3104 = EDGE_CURVE('',#2489,#2490,#1397,.T.) ;
#3105 = EDGE_CURVE('',#2490,#2491,#271,.T.) ;
#3106 = EDGE_CURVE('',#2491,#2492,#1398,.T.) ;
#3107 = EDGE_CURVE('',#2489,#2492,#272,.T.) ;
#3108 = EDGE_CURVE('',#2490,#2493,#2120,.T.) ;
#3109 = EDGE_CURVE('',#2493,#2494,#273,.T.) ;
#3110 = EDGE_CURVE('',#2494,#2491,#2121,.T.) ;
#3111 = EDGE_CURVE('',#2493,#2495,#1399,.T.) ;
#3112 = EDGE_CURVE('',#2495,#2496,#274,.T.) ;
#3113 = EDGE_CURVE('',#2496,#2494,#1400,.T.) ;
#3114 = EDGE_CURVE('',#2495,#2497,#2122,.T.) ;
#3115 = EDGE_CURVE('',#2497,#2498,#275,.T.) ;
#3116 = EDGE_CURVE('',#2498,#2496,#2123,.T.) ;
#3117 = EDGE_CURVE('',#2497,#2499,#1401,.T.) ;
#3118 = EDGE_CURVE('',#2499,#2500,#276,.T.) ;
#3119 = EDGE_CURVE('',#2500,#2498,#1402,.T.) ;
#3120 = EDGE_CURVE('',#2501,#2502,#277,.T.) ;
#3121 = EDGE_CURVE('',#2502,#2503,#2124,.T.) ;
#3122 = EDGE_CURVE('',#2503,#2504,#278,.T.) ;
#3123 = EDGE_CURVE('',#2504,#2501,#2125,.T.) ;
#3124 = EDGE_CURVE('',#2505,#2504,#1403,.T.) ;
#3125 = EDGE_CURVE('',#2503,#2506,#1404,.T.) ;
#3126 = EDGE_CURVE('',#2506,#2505,#279,.T.) ;
#3127 = EDGE_CURVE('',#2499,#2507,#2126,.T.) ;
#3128 = EDGE_CURVE('',#2507,#2508,#280,.T.) ;
#3129 = EDGE_CURVE('',#2508,#2500,#2127,.T.) ;
#3130 = EDGE_CURVE('',#2501,#2509,#1405,.T.) ;
#3131 = EDGE_CURVE('',#2509,#2510,#281,.T.) ;
#3132 = EDGE_CURVE('',#2510,#2502,#1406,.T.) ;
#3133 = EDGE_CURVE('',#2507,#2511,#2128,.T.) ;
#3134 = EDGE_CURVE('',#2511,#2512,#282,.T.) ;
#3135 = EDGE_CURVE('',#2512,#2508,#2129,.T.) ;
#3136 = EDGE_CURVE('',#2513,#2514,#283,.T.) ;
#3137 = EDGE_CURVE('',#2514,#2515,#1407,.T.) ;
#3138 = EDGE_CURVE('',#2515,#2516,#284,.T.) ;
#3139 = EDGE_CURVE('',#2516,#2513,#1408,.T.) ;
#3140 = EDGE_CURVE('',#2517,#2518,#1409,.T.) ;
#3141 = EDGE_CURVE('',#2518,#2519,#285,.T.) ;
#3142 = EDGE_CURVE('',#2519,#2520,#1410,.T.) ;
#3143 = EDGE_CURVE('',#2520,#2517,#394,.T.) ;
#3144 = EDGE_CURVE('',#2515,#2521,#2130,.T.) ;
#3145 = EDGE_CURVE('',#2521,#2522,#286,.T.) ;
#3146 = EDGE_CURVE('',#2522,#2516,#2131,.T.) ;
#3147 = EDGE_CURVE('',#2518,#2523,#2132,.T.) ;
#3148 = EDGE_CURVE('',#2523,#2524,#287,.T.) ;
#3149 = EDGE_CURVE('',#2524,#2519,#2133,.T.) ;
#3150 = EDGE_CURVE('',#2521,#2525,#2134,.T.) ;
#3151 = EDGE_CURVE('',#2525,#2526,#288,.T.) ;
#3152 = EDGE_CURVE('',#2526,#2522,#2135,.T.) ;
#3153 = EDGE_CURVE('',#2527,#2528,#289,.T.) ;
#3154 = EDGE_CURVE('',#2528,#2529,#2136,.T.) ;
#3155 = EDGE_CURVE('',#2529,#2530,#2137,.T.) ;
#3156 = EDGE_CURVE('',#2530,#2527,#2138,.T.) ;
#3157 = EDGE_CURVE('',#2525,#2528,#1411,.T.) ;
#3158 = EDGE_CURVE('',#2527,#2526,#1412,.T.) ;
#3159 = EDGE_CURVE('',#2523,#2530,#1413,.T.) ;
#3160 = EDGE_CURVE('',#2529,#2524,#1414,.T.) ;
#3161 = EDGE_CURVE('',#2531,#2517,#1415,.T.) ;
#3162 = EDGE_CURVE('',#2520,#2532,#1416,.T.) ;
#3163 = EDGE_CURVE('',#2532,#2531,#290,.T.) ;
#3164 = EDGE_CURVE('',#2533,#2534,#291,.T.) ;
#3165 = EDGE_CURVE('',#2534,#2514,#2139,.T.) ;
#3166 = EDGE_CURVE('',#2513,#2533,#2140,.T.) ;
#3167 = EDGE_CURVE('',#2535,#2531,#2141,.T.) ;
#3168 = EDGE_CURVE('',#2532,#2536,#2142,.T.) ;
#3169 = EDGE_CURVE('',#2536,#2535,#292,.T.) ;
#3170 = EDGE_CURVE('',#2511,#2534,#1417,.T.) ;
#3171 = EDGE_CURVE('',#2533,#2512,#1418,.T.) ;
#3172 = EDGE_CURVE('',#2509,#2537,#2143,.T.) ;
#3173 = EDGE_CURVE('',#2537,#2538,#2144,.T.) ;
#3174 = EDGE_CURVE('',#2538,#2510,#2145,.T.) ;
#3175 = EDGE_CURVE('',#2536,#2538,#1419,.T.) ;
#3176 = EDGE_CURVE('',#2537,#2535,#1420,.T.) ;
#3177 = EDGE_CURVE('',#2539,#2505,#2146,.T.) ;
#3178 = EDGE_CURVE('',#2506,#2540,#2147,.T.) ;
#3179 = EDGE_CURVE('',#2540,#2539,#293,.T.) ;
#3180 = EDGE_CURVE('',#2541,#2539,#1421,.T.) ;
#3181 = EDGE_CURVE('',#2540,#2542,#1422,.T.) ;
#3182 = EDGE_CURVE('',#2542,#2541,#294,.T.) ;
#3183 = EDGE_CURVE('',#2542,#2543,#2148,.T.) ;
#3184 = EDGE_CURVE('',#2543,#2544,#295,.T.) ;
#3185 = EDGE_CURVE('',#2544,#2541,#2149,.T.) ;
#3186 = EDGE_CURVE('',#2545,#2544,#1423,.T.) ;
#3187 = EDGE_CURVE('',#2543,#2546,#1424,.T.) ;
#3188 = EDGE_CURVE('',#2546,#2545,#296,.T.) ;
#3189 = EDGE_CURVE('',#2492,#2545,#2150,.T.) ;
#3190 = EDGE_CURVE('',#2546,#2489,#2151,.T.) ;
#3191 = EDGE_CURVE('',#2547,#2492,#1425,.T.) ;
#3192 = EDGE_CURVE('',#2548,#2547,#2152,.T.) ;
#3193 = EDGE_CURVE('',#2548,#2545,#1426,.T.) ;
#3194 = EDGE_CURVE('',#2549,#2491,#1427,.T.) ;
#3195 = EDGE_CURVE('',#2547,#2549,#1428,.T.) ;
#3196 = EDGE_CURVE('',#2550,#2494,#1429,.T.) ;
#3197 = EDGE_CURVE('',#2549,#2550,#2153,.T.) ;
#3198 = EDGE_CURVE('',#2551,#2496,#1430,.T.) ;
#3199 = EDGE_CURVE('',#2550,#2551,#1431,.T.) ;
#3200 = EDGE_CURVE('',#2552,#2498,#1432,.T.) ;
#3201 = EDGE_CURVE('',#2551,#2552,#2154,.T.) ;
#3202 = EDGE_CURVE('',#2553,#2500,#1433,.T.) ;
#3203 = EDGE_CURVE('',#2552,#2553,#1434,.T.) ;
#3204 = EDGE_CURVE('',#2554,#2508,#1435,.T.) ;
#3205 = EDGE_CURVE('',#2553,#2554,#2155,.T.) ;
#3206 = EDGE_CURVE('',#2555,#2512,#1436,.T.) ;
#3207 = EDGE_CURVE('',#2554,#2555,#2156,.T.) ;
#3208 = EDGE_CURVE('',#2556,#2533,#1437,.T.) ;
#3209 = EDGE_CURVE('',#2555,#2556,#1438,.T.) ;
#3210 = EDGE_CURVE('',#2557,#2513,#1439,.T.) ;
#3211 = EDGE_CURVE('',#2556,#2557,#2157,.T.) ;
#3212 = EDGE_CURVE('',#2558,#2516,#1440,.T.) ;
#3213 = EDGE_CURVE('',#2557,#2558,#1441,.T.) ;
#3214 = EDGE_CURVE('',#2559,#2522,#1442,.T.) ;
#3215 = EDGE_CURVE('',#2558,#2559,#2158,.T.) ;
#3216 = EDGE_CURVE('',#2560,#2526,#1443,.T.) ;
#3217 = EDGE_CURVE('',#2559,#2560,#2159,.T.) ;
#3218 = EDGE_CURVE('',#2561,#2527,#1444,.T.) ;
#3219 = EDGE_CURVE('',#2560,#2561,#1445,.T.) ;
#3220 = EDGE_CURVE('',#2562,#2530,#1446,.T.) ;
#3221 = EDGE_CURVE('',#2561,#2562,#2160,.T.) ;
#3222 = EDGE_CURVE('',#2563,#2564,#1447,.T.) ;
#3223 = EDGE_CURVE('',#2565,#2563,#2161,.T.) ;
#3224 = EDGE_CURVE('',#2566,#2565,#1448,.T.) ;
#3225 = EDGE_CURVE('',#2564,#2566,#2162,.T.) ;
#3226 = EDGE_CURVE('',#2567,#2567,#2163,.T.) ;
#3227 = EDGE_CURVE('',#2568,#2569,#2164,.T.) ;
#3228 = EDGE_CURVE('',#2569,#2548,#297,.T.) ;
#3229 = EDGE_CURVE('',#2568,#2547,#298,.T.) ;
#3230 = EDGE_CURVE('',#2569,#2570,#1449,.T.) ;
#3231 = EDGE_CURVE('',#2570,#2571,#299,.T.) ;
#3232 = EDGE_CURVE('',#2571,#2548,#1450,.T.) ;
#3233 = EDGE_CURVE('',#2570,#2572,#2165,.T.) ;
#3234 = EDGE_CURVE('',#2572,#2573,#300,.T.) ;
#3235 = EDGE_CURVE('',#2573,#2571,#2166,.T.) ;
#3236 = EDGE_CURVE('',#2572,#2574,#1451,.T.) ;
#3237 = EDGE_CURVE('',#2574,#2575,#301,.T.) ;
#3238 = EDGE_CURVE('',#2575,#2573,#1452,.T.) ;
#3239 = EDGE_CURVE('',#2574,#2576,#2167,.T.) ;
#3240 = EDGE_CURVE('',#2576,#2577,#302,.T.) ;
#3241 = EDGE_CURVE('',#2577,#2575,#2168,.T.) ;
#3242 = EDGE_CURVE('',#2556,#2578,#303,.T.) ;
#3243 = EDGE_CURVE('',#2578,#2579,#1453,.T.) ;
#3244 = EDGE_CURVE('',#2579,#2555,#304,.T.) ;
#3245 = EDGE_CURVE('',#2580,#2581,#305,.T.) ;
#3246 = EDGE_CURVE('',#2581,#2582,#2169,.T.) ;
#3247 = EDGE_CURVE('',#2582,#2583,#2170,.T.) ;
#3248 = EDGE_CURVE('',#2583,#2580,#2171,.T.) ;
#3249 = EDGE_CURVE('',#2584,#2583,#1454,.T.) ;
#3250 = EDGE_CURVE('',#2582,#2585,#1455,.T.) ;
#3251 = EDGE_CURVE('',#2585,#2584,#306,.T.) ;
#3252 = EDGE_CURVE('',#2557,#2586,#307,.T.) ;
#3253 = EDGE_CURVE('',#2586,#2578,#2172,.T.) ;
#3254 = EDGE_CURVE('',#2585,#2587,#2173,.T.) ;
#3255 = EDGE_CURVE('',#2587,#2588,#308,.T.) ;
#3256 = EDGE_CURVE('',#2588,#2584,#2174,.T.) ;
#3257 = EDGE_CURVE('',#2587,#2589,#1456,.T.) ;
#3258 = EDGE_CURVE('',#2589,#2590,#395,.T.) ;
#3259 = EDGE_CURVE('',#2590,#2588,#1457,.T.) ;
#3260 = EDGE_CURVE('',#2591,#2561,#309,.T.) ;
#3261 = EDGE_CURVE('',#2562,#2592,#2175,.T.) ;
#3262 = EDGE_CURVE('',#2592,#2591,#2176,.T.) ;
#3263 = EDGE_CURVE('',#2593,#2594,#310,.T.) ;
#3264 = EDGE_CURVE('',#2594,#2592,#1458,.T.) ;
#3265 = EDGE_CURVE('',#2562,#2593,#1459,.T.) ;
#3266 = EDGE_CURVE('',#2591,#2595,#1460,.T.) ;
#3267 = EDGE_CURVE('',#2595,#2560,#311,.T.) ;
#3268 = EDGE_CURVE('',#2596,#2597,#312,.T.) ;
#3269 = EDGE_CURVE('',#2597,#2594,#2177,.T.) ;
#3270 = EDGE_CURVE('',#2593,#2596,#2178,.T.) ;
#3271 = EDGE_CURVE('',#2595,#2598,#2179,.T.) ;
#3272 = EDGE_CURVE('',#2598,#2559,#313,.T.) ;
#3273 = EDGE_CURVE('',#2589,#2597,#1461,.T.) ;
#3274 = EDGE_CURVE('',#2596,#2590,#1462,.T.) ;
#3275 = EDGE_CURVE('',#2598,#2599,#2180,.T.) ;
#3276 = EDGE_CURVE('',#2599,#2558,#314,.T.) ;
#3277 = EDGE_CURVE('',#2599,#2586,#1463,.T.) ;
#3278 = EDGE_CURVE('',#2600,#2601,#315,.T.) ;
#3279 = EDGE_CURVE('',#2601,#2581,#1464,.T.) ;
#3280 = EDGE_CURVE('',#2580,#2600,#1465,.T.) ;
#3281 = EDGE_CURVE('',#2579,#2602,#2181,.T.) ;
#3282 = EDGE_CURVE('',#2602,#2554,#316,.T.) ;
#3283 = EDGE_CURVE('',#2576,#2603,#1466,.T.) ;
#3284 = EDGE_CURVE('',#2603,#2604,#317,.T.) ;
#3285 = EDGE_CURVE('',#2604,#2577,#1467,.T.) ;
#3286 = EDGE_CURVE('',#2600,#2604,#2182,.T.) ;
#3287 = EDGE_CURVE('',#2603,#2601,#2183,.T.) ;
#3288 = EDGE_CURVE('',#2602,#2605,#2184,.T.) ;
#3289 = EDGE_CURVE('',#2605,#2553,#318,.T.) ;
#3290 = EDGE_CURVE('',#2605,#2606,#1468,.T.) ;
#3291 = EDGE_CURVE('',#2606,#2552,#319,.T.) ;
#3292 = EDGE_CURVE('',#2606,#2607,#2185,.T.) ;
#3293 = EDGE_CURVE('',#2607,#2551,#320,.T.) ;
#3294 = EDGE_CURVE('',#2607,#2608,#1469,.T.) ;
#3295 = EDGE_CURVE('',#2608,#2550,#321,.T.) ;
#3296 = EDGE_CURVE('',#2608,#2609,#2186,.T.) ;
#3297 = EDGE_CURVE('',#2609,#2549,#322,.T.) ;
#3298 = EDGE_CURVE('',#2609,#2568,#1470,.T.) ;
#3299 = EDGE_CURVE('',#2571,#2544,#1471,.T.) ;
#3300 = EDGE_CURVE('',#2573,#2541,#1472,.T.) ;
#3301 = EDGE_CURVE('',#2575,#2539,#1473,.T.) ;
#3302 = EDGE_CURVE('',#2577,#2505,#1474,.T.) ;
#3303 = EDGE_CURVE('',#2604,#2504,#1475,.T.) ;
#3304 = EDGE_CURVE('',#2600,#2501,#1476,.T.) ;
#3305 = EDGE_CURVE('',#2580,#2509,#1477,.T.) ;
#3306 = EDGE_CURVE('',#2583,#2537,#1478,.T.) ;
#3307 = EDGE_CURVE('',#2584,#2535,#1479,.T.) ;
#3308 = EDGE_CURVE('',#2588,#2531,#1480,.T.) ;
#3309 = EDGE_CURVE('',#2590,#2517,#1481,.T.) ;
#3310 = EDGE_CURVE('',#2596,#2518,#1482,.T.) ;
#3311 = EDGE_CURVE('',#2593,#2523,#1483,.T.) ;
#3312 = EDGE_CURVE('',#2610,#2611,#2187,.T.) ;
#3313 = EDGE_CURVE('',#2612,#2610,#1484,.T.) ;
#3314 = EDGE_CURVE('',#2613,#2612,#2188,.T.) ;
#3315 = EDGE_CURVE('',#2611,#2613,#1485,.T.) ;
#3316 = EDGE_CURVE('',#2614,#2614,#2189,.T.) ;
#3317 = EDGE_CURVE('',#2564,#2615,#323,.T.) ;
#3318 = EDGE_CURVE('',#2615,#2616,#1486,.T.) ;
#3319 = EDGE_CURVE('',#2563,#2616,#324,.T.) ;
#3320 = EDGE_CURVE('',#2566,#2617,#325,.T.) ;
#3321 = EDGE_CURVE('',#2617,#2615,#2190,.T.) ;
#3322 = EDGE_CURVE('',#2565,#2618,#326,.T.) ;
#3323 = EDGE_CURVE('',#2618,#2617,#1487,.T.) ;
#3324 = EDGE_CURVE('',#2616,#2618,#2191,.T.) ;
#3325 = EDGE_CURVE('',#2619,#2616,#1488,.T.) ;
#3326 = EDGE_CURVE('',#2620,#2619,#2192,.T.) ;
#3327 = EDGE_CURVE('',#2620,#2618,#1489,.T.) ;
#3328 = EDGE_CURVE('',#2621,#2615,#1490,.T.) ;
#3329 = EDGE_CURVE('',#2619,#2621,#1491,.T.) ;
#3330 = EDGE_CURVE('',#2621,#2622,#2193,.T.) ;
#3331 = EDGE_CURVE('',#2622,#2613,#327,.T.) ;
#3332 = EDGE_CURVE('',#2612,#2621,#328,.T.) ;
#3333 = EDGE_CURVE('',#2611,#2620,#329,.T.) ;
#3334 = EDGE_CURVE('',#2610,#2619,#330,.T.) ;
#3335 = EDGE_CURVE('',#2622,#2620,#1492,.T.) ;
#3336 = EDGE_CURVE('',#2567,#2614,#1493,.T.) ;
#3337 = EDGE_CURVE('',#2622,#2617,#1494,.T.) ;
#3338 = EDGE_CURVE('',#2623,#2623,#2194,.T.) ;
#3339 = EDGE_CURVE('',#2624,#2624,#2195,.T.) ;
#3340 = EDGE_CURVE('',#2624,#2623,#1495,.T.) ;
#3341 = EDGE_CURVE('',#2625,#2625,#2196,.T.) ;
#3342 = EDGE_CURVE('',#2625,#2624,#1496,.T.) ;
#3343 = EDGE_CURVE('',#2626,#2626,#2197,.T.) ;
#3344 = EDGE_CURVE('',#2626,#2625,#1497,.T.) ;
#3345 = EDGE_CURVE('',#2627,#2627,#2198,.T.) ;
#3346 = EDGE_CURVE('',#2628,#2628,#2199,.T.) ;
#3347 = EDGE_CURVE('',#2628,#2627,#1498,.T.) ;
#3348 = EDGE_CURVE('',#2629,#2629,#2200,.T.) ;
#3349 = EDGE_CURVE('',#2630,#2630,#2201,.T.) ;
#3350 = EDGE_CURVE('',#2630,#2629,#1499,.T.) ;
#3351 = EDGE_CURVE('',#2631,#2631,#2202,.T.) ;
#3352 = EDGE_CURVE('',#2631,#2630,#1500,.T.) ;
#3353 = EDGE_CURVE('',#2632,#2632,#2203,.T.) ;
#3354 = EDGE_CURVE('',#2632,#2631,#1501,.T.) ;
#3355 = EDGE_CURVE('',#2633,#2633,#2204,.T.) ;
#3356 = EDGE_CURVE('',#2634,#2634,#2205,.T.) ;
#3357 = EDGE_CURVE('',#2634,#2633,#1502,.T.) ;
#3358 = EDGE_CURVE('',#2635,#2635,#2206,.T.) ;
#3359 = EDGE_CURVE('',#2636,#2636,#2207,.T.) ;
#3360 = EDGE_CURVE('',#2636,#2635,#1503,.T.) ;
#3361 = EDGE_CURVE('',#2637,#2637,#2208,.T.) ;
#3362 = EDGE_CURVE('',#2637,#2636,#1504,.T.) ;
#3363 = EDGE_CURVE('',#2638,#2638,#2209,.T.) ;
#3364 = EDGE_CURVE('',#2638,#2637,#1505,.T.) ;
#3365 = EDGE_CURVE('',#2639,#2639,#2210,.T.) ;
#3366 = EDGE_CURVE('',#2639,#2640,#1506,.T.) ;
#3367 = EDGE_CURVE('',#2640,#2640,#2211,.T.) ;
#3368 = EDGE_CURVE('',#2641,#2642,#1507,.T.) ;
#3369 = EDGE_CURVE('',#2642,#2643,#1508,.T.) ;
#3370 = EDGE_CURVE('',#2644,#2643,#1509,.T.) ;
#3371 = EDGE_CURVE('',#2641,#2644,#1510,.T.) ;
#3372 = EDGE_CURVE('',#2645,#2641,#1511,.T.) ;
#3373 = EDGE_CURVE('',#2646,#2644,#1512,.T.) ;
#3374 = EDGE_CURVE('',#2645,#2646,#1513,.T.) ;
#3375 = EDGE_CURVE('',#2647,#2645,#1514,.T.) ;
#3376 = EDGE_CURVE('',#2648,#2646,#1515,.T.) ;
#3377 = EDGE_CURVE('',#2647,#2648,#1516,.T.) ;
#3378 = EDGE_CURVE('',#2649,#2647,#1517,.T.) ;
#3379 = EDGE_CURVE('',#2650,#2648,#1518,.T.) ;
#3380 = EDGE_CURVE('',#2649,#2650,#1519,.T.) ;
#3381 = EDGE_CURVE('',#2651,#2649,#1520,.T.) ;
#3382 = EDGE_CURVE('',#2652,#2650,#1521,.T.) ;
#3383 = EDGE_CURVE('',#2651,#2652,#1522,.T.) ;
#3384 = EDGE_CURVE('',#2653,#2651,#1523,.T.) ;
#3385 = EDGE_CURVE('',#2654,#2652,#1524,.T.) ;
#3386 = EDGE_CURVE('',#2653,#2654,#1525,.T.) ;
#3387 = EDGE_CURVE('',#2655,#2653,#1526,.T.) ;
#3388 = EDGE_CURVE('',#2656,#2654,#1527,.T.) ;
#3389 = EDGE_CURVE('',#2655,#2656,#1528,.T.) ;
#3390 = EDGE_CURVE('',#2657,#2655,#1529,.T.) ;
#3391 = EDGE_CURVE('',#2658,#2656,#1530,.T.) ;
#3392 = EDGE_CURVE('',#2657,#2658,#1531,.T.) ;
#3393 = EDGE_CURVE('',#2642,#2657,#1532,.T.) ;
#3394 = EDGE_CURVE('',#2643,#2658,#1533,.T.) ;
#3395 = EDGE_CURVE('',#2659,#2660,#1534,.T.) ;
#3396 = EDGE_CURVE('',#2659,#2661,#1535,.T.) ;
#3397 = EDGE_CURVE('',#2661,#2662,#1536,.T.) ;
#3398 = EDGE_CURVE('',#2660,#2662,#1537,.T.) ;
#3399 = EDGE_CURVE('',#2660,#2663,#1538,.T.) ;
#3400 = EDGE_CURVE('',#2662,#2664,#1539,.T.) ;
#3401 = EDGE_CURVE('',#2663,#2664,#1540,.T.) ;
#3402 = EDGE_CURVE('',#2663,#2665,#1541,.T.) ;
#3403 = EDGE_CURVE('',#2664,#2666,#1542,.T.) ;
#3404 = EDGE_CURVE('',#2665,#2666,#1543,.T.) ;
#3405 = EDGE_CURVE('',#2665,#2667,#1544,.T.) ;
#3406 = EDGE_CURVE('',#2666,#2668,#1545,.T.) ;
#3407 = EDGE_CURVE('',#2668,#2667,#1546,.T.) ;
#3408 = EDGE_CURVE('',#2669,#2659,#1547,.T.) ;
#3409 = EDGE_CURVE('',#2669,#2670,#1548,.T.) ;
#3410 = EDGE_CURVE('',#2670,#2661,#1549,.T.) ;
#3411 = EDGE_CURVE('',#2667,#2669,#1550,.T.) ;
#3412 = EDGE_CURVE('',#2668,#2670,#1551,.T.) ;
#3413 = EDGE_CURVE('',#2671,#2671,#2212,.T.) ;
#3414 = EDGE_CURVE('',#2672,#2672,#2213,.T.) ;
#3415 = EDGE_CURVE('',#2672,#2671,#1552,.T.) ;
#3416 = EDGE_CURVE('',#2673,#2673,#2214,.T.) ;
#3417 = EDGE_CURVE('',#2673,#2672,#1553,.T.) ;
#3418 = EDGE_CURVE('',#2674,#2674,#2215,.T.) ;
#3419 = EDGE_CURVE('',#2674,#2673,#1554,.T.) ;
#3420 = EDGE_CURVE('',#2675,#2675,#2216,.T.) ;
#3421 = EDGE_CURVE('',#2675,#2674,#1555,.T.) ;
#3422 = EDGE_CURVE('',#2676,#2676,#2217,.T.) ;
#3423 = EDGE_CURVE('',#2676,#2675,#1556,.T.) ;
#3424 = EDGE_CURVE('',#2677,#2677,#2218,.T.) ;
#3425 = EDGE_CURVE('',#2677,#2678,#1557,.T.) ;
#3426 = EDGE_CURVE('',#2679,#2678,#331,.T.) ;
#3427 = EDGE_CURVE('',#2680,#2679,#332,.T.) ;
#3428 = EDGE_CURVE('',#2681,#2680,#333,.T.) ;
#3429 = EDGE_CURVE('',#2678,#2681,#334,.T.) ;
#3430 = EDGE_CURVE('',#2682,#2677,#1558,.T.) ;
#3431 = EDGE_CURVE('',#2683,#2683,#2219,.T.) ;
#3432 = EDGE_CURVE('',#2683,#2684,#2220,.T.) ;
#3433 = EDGE_CURVE('',#2681,#2684,#2221,.T.) ;
#3434 = EDGE_CURVE('',#2684,#2679,#2222,.T.) ;
#3435 = EDGE_CURVE('',#2684,#2685,#2223,.T.) ;
#3436 = EDGE_CURVE('',#2686,#2685,#2224,.T.) ;
#3437 = EDGE_CURVE('',#2686,#2687,#335,.T.) ;
#3438 = EDGE_CURVE('',#2685,#2687,#2225,.T.) ;
#3439 = EDGE_CURVE('',#2688,#2688,#2226,.T.) ;
#3440 = EDGE_CURVE('',#2688,#2689,#1559,.T.) ;
#3441 = EDGE_CURVE('',#2687,#2689,#336,.T.) ;
#3442 = EDGE_CURVE('',#2689,#2686,#2227,.T.) ;
#3443 = EDGE_CURVE('',#2690,#2688,#1560,.T.) ;
#3444 = EDGE_CURVE('',#2691,#2691,#2228,.T.) ;
#3445 = EDGE_CURVE('',#2691,#2683,#2229,.T.) ;
#3446 = EDGE_CURVE('',#2685,#2691,#2230,.T.) ;
#3447 = EDGE_CURVE('',#2692,#2692,#2231,.T.) ;
#3448 = EDGE_CURVE('',#2692,#2693,#1561,.T.) ;
#3449 = EDGE_CURVE('',#2693,#2693,#2232,.T.) ;
#3450 = EDGE_CURVE('',#2694,#2694,#2233,.T.) ;
#3451 = EDGE_CURVE('',#2695,#2695,#2234,.T.) ;
#3452 = EDGE_CURVE('',#2695,#2694,#1562,.T.) ;
#3453 = EDGE_CURVE('',#2696,#2696,#2235,.T.) ;
#3454 = EDGE_CURVE('',#2696,#2697,#1563,.T.) ;
#3455 = EDGE_CURVE('',#2697,#2697,#2236,.T.) ;
#3456 = EDGE_CURVE('',#2698,#2698,#2237,.T.) ;
#3457 = EDGE_CURVE('',#2699,#2699,#2238,.T.) ;
#3458 = EDGE_CURVE('',#2699,#2698,#1564,.T.) ;
#3459 = EDGE_CURVE('',#2700,#2700,#2239,.T.) ;
#3460 = EDGE_CURVE('',#2700,#2701,#1565,.T.) ;
#3461 = EDGE_CURVE('',#2701,#2701,#2240,.T.) ;
#3462 = EDGE_CURVE('',#2702,#2702,#2241,.T.) ;
#3463 = EDGE_CURVE('',#2703,#2703,#2242,.T.) ;
#3464 = EDGE_CURVE('',#2703,#2702,#1566,.T.) ;
#3465 = EDGE_CURVE('',#2704,#2705,#2243,.T.) ;
#3466 = EDGE_CURVE('',#2704,#2706,#1567,.T.) ;
#3467 = EDGE_CURVE('',#2707,#2706,#2244,.T.) ;
#3468 = EDGE_CURVE('',#2705,#2707,#1568,.T.) ;
#3469 = EDGE_CURVE('',#2708,#2705,#1569,.T.) ;
#3470 = EDGE_CURVE('',#2709,#2707,#1570,.T.) ;
#3471 = EDGE_CURVE('',#2708,#2709,#1571,.T.) ;
#3472 = EDGE_CURVE('',#2710,#2708,#1572,.T.) ;
#3473 = EDGE_CURVE('',#2711,#2709,#1573,.T.) ;
#3474 = EDGE_CURVE('',#2710,#2711,#1574,.T.) ;
#3475 = EDGE_CURVE('',#2710,#2712,#2245,.T.) ;
#3476 = EDGE_CURVE('',#2713,#2711,#2246,.T.) ;
#3477 = EDGE_CURVE('',#2712,#2713,#1575,.T.) ;
#3478 = EDGE_CURVE('',#2714,#2712,#1576,.T.) ;
#3479 = EDGE_CURVE('',#2715,#2713,#1577,.T.) ;
#3480 = EDGE_CURVE('',#2714,#2715,#1578,.T.) ;
#3481 = EDGE_CURVE('',#2716,#2714,#2247,.T.) ;
#3482 = EDGE_CURVE('',#2717,#2715,#2248,.T.) ;
#3483 = EDGE_CURVE('',#2716,#2717,#1579,.T.) ;
#3484 = EDGE_CURVE('',#2718,#2716,#2249,.T.) ;
#3485 = EDGE_CURVE('',#2719,#2717,#2250,.T.) ;
#3486 = EDGE_CURVE('',#2718,#2719,#1580,.T.) ;
#3487 = EDGE_CURVE('',#2704,#2718,#1581,.T.) ;
#3488 = EDGE_CURVE('',#2706,#2719,#1582,.T.) ;
#3489 = EDGE_CURVE('',#2720,#2720,#2251,.T.) ;
#3490 = EDGE_CURVE('',#2720,#2721,#1583,.T.) ;
#3491 = EDGE_CURVE('',#2721,#2721,#2252,.T.) ;
#3492 = EDGE_CURVE('',#2722,#2723,#2253,.T.) ;
#3493 = EDGE_CURVE('',#2722,#2724,#1584,.T.) ;
#3494 = EDGE_CURVE('',#2725,#2724,#2254,.T.) ;
#3495 = EDGE_CURVE('',#2723,#2725,#1585,.T.) ;
#3496 = EDGE_CURVE('',#2726,#2723,#1586,.T.) ;
#3497 = EDGE_CURVE('',#2727,#2725,#1587,.T.) ;
#3498 = EDGE_CURVE('',#2726,#2727,#1588,.T.) ;
#3499 = EDGE_CURVE('',#2728,#2726,#2255,.T.) ;
#3500 = EDGE_CURVE('',#2729,#2727,#2256,.T.) ;
#3501 = EDGE_CURVE('',#2728,#2729,#1589,.T.) ;
#3502 = EDGE_CURVE('',#2730,#2728,#2257,.T.) ;
#3503 = EDGE_CURVE('',#2731,#2729,#2258,.T.) ;
#3504 = EDGE_CURVE('',#2730,#2731,#1590,.T.) ;
#3505 = EDGE_CURVE('',#2732,#2730,#1591,.T.) ;
#3506 = EDGE_CURVE('',#2733,#2731,#1592,.T.) ;
#3507 = EDGE_CURVE('',#2732,#2733,#1593,.T.) ;
#3508 = EDGE_CURVE('',#2734,#2732,#2259,.T.) ;
#3509 = EDGE_CURVE('',#2735,#2733,#2260,.T.) ;
#3510 = EDGE_CURVE('',#2734,#2735,#1594,.T.) ;
#3511 = EDGE_CURVE('',#2736,#2734,#1595,.T.) ;
#3512 = EDGE_CURVE('',#2737,#2735,#1596,.T.) ;
#3513 = EDGE_CURVE('',#2736,#2737,#1597,.T.) ;
#3514 = EDGE_CURVE('',#2738,#2736,#2261,.T.) ;
#3515 = EDGE_CURVE('',#2739,#2737,#2262,.T.) ;
#3516 = EDGE_CURVE('',#2738,#2739,#1598,.T.) ;
#3517 = EDGE_CURVE('',#2740,#2738,#2263,.T.) ;
#3518 = EDGE_CURVE('',#2741,#2739,#2264,.T.) ;
#3519 = EDGE_CURVE('',#2740,#2741,#1599,.T.) ;
#3520 = EDGE_CURVE('',#2722,#2740,#1600,.T.) ;
#3521 = EDGE_CURVE('',#2724,#2741,#1601,.T.) ;
#3522 = EDGE_CURVE('',#2742,#2742,#2265,.T.) ;
#3523 = EDGE_CURVE('',#2742,#2743,#1602,.T.) ;
#3524 = EDGE_CURVE('',#2743,#2743,#2266,.T.) ;
#3525 = EDGE_CURVE('',#2744,#2744,#2267,.T.) ;
#3526 = EDGE_CURVE('',#2745,#2745,#2268,.T.) ;
#3527 = EDGE_CURVE('',#2745,#2744,#1603,.T.) ;
#3528 = ORIENTED_EDGE('',*,*,#2746,.F.) ;
#3529 = ORIENTED_EDGE('',*,*,#2747,.T.) ;
#3530 = ORIENTED_EDGE('',*,*,#2748,.F.) ;
#3531 = ORIENTED_EDGE('',*,*,#2747,.F.) ;
#3532 = ORIENTED_EDGE('',*,*,#2749,.F.) ;
#3533 = ORIENTED_EDGE('',*,*,#2750,.T.) ;
#3534 = ORIENTED_EDGE('',*,*,#2751,.F.) ;
#3535 = ORIENTED_EDGE('',*,*,#2750,.F.) ;
#3536 = ORIENTED_EDGE('',*,*,#2752,.F.) ;
#3537 = ORIENTED_EDGE('',*,*,#2753,.T.) ;
#3538 = ORIENTED_EDGE('',*,*,#2754,.F.) ;
#3539 = ORIENTED_EDGE('',*,*,#2753,.F.) ;
#3540 = ORIENTED_EDGE('',*,*,#2755,.F.) ;
#3541 = ORIENTED_EDGE('',*,*,#2756,.F.) ;
#3542 = ORIENTED_EDGE('',*,*,#2757,.T.) ;
#3543 = ORIENTED_EDGE('',*,*,#2758,.T.) ;
#3544 = ORIENTED_EDGE('',*,*,#2759,.F.) ;
#3545 = ORIENTED_EDGE('',*,*,#2760,.F.) ;
#3546 = ORIENTED_EDGE('',*,*,#2761,.F.) ;
#3547 = ORIENTED_EDGE('',*,*,#2758,.F.) ;
#3548 = ORIENTED_EDGE('',*,*,#2762,.F.) ;
#3549 = ORIENTED_EDGE('',*,*,#2763,.F.) ;
#3550 = ORIENTED_EDGE('',*,*,#2764,.F.) ;
#3551 = ORIENTED_EDGE('',*,*,#2765,.F.) ;
#3552 = ORIENTED_EDGE('',*,*,#2766,.F.) ;
#3553 = ORIENTED_EDGE('',*,*,#2767,.F.) ;
#3554 = ORIENTED_EDGE('',*,*,#2752,.T.) ;
#3555 = ORIENTED_EDGE('',*,*,#2768,.F.) ;
#3556 = ORIENTED_EDGE('',*,*,#2769,.T.) ;
#3557 = ORIENTED_EDGE('',*,*,#2762,.T.) ;
#3558 = ORIENTED_EDGE('',*,*,#2757,.F.) ;
#3559 = ORIENTED_EDGE('',*,*,#2770,.F.) ;
#3560 = ORIENTED_EDGE('',*,*,#2771,.T.) ;
#3561 = ORIENTED_EDGE('',*,*,#2763,.T.) ;
#3562 = ORIENTED_EDGE('',*,*,#2769,.F.) ;
#3563 = ORIENTED_EDGE('',*,*,#2772,.F.) ;
#3564 = ORIENTED_EDGE('',*,*,#2773,.T.) ;
#3565 = ORIENTED_EDGE('',*,*,#2764,.T.) ;
#3566 = ORIENTED_EDGE('',*,*,#2771,.F.) ;
#3567 = ORIENTED_EDGE('',*,*,#2748,.T.) ;
#3568 = ORIENTED_EDGE('',*,*,#2774,.F.) ;
#3569 = ORIENTED_EDGE('',*,*,#2765,.T.) ;
#3570 = ORIENTED_EDGE('',*,*,#2773,.F.) ;
#3571 = ORIENTED_EDGE('',*,*,#2775,.F.) ;
#3572 = ORIENTED_EDGE('',*,*,#2776,.F.) ;
#3573 = ORIENTED_EDGE('',*,*,#2777,.F.) ;
#3574 = ORIENTED_EDGE('',*,*,#2778,.F.) ;
#3575 = ORIENTED_EDGE('',*,*,#2775,.T.) ;
#3576 = ORIENTED_EDGE('',*,*,#2772,.T.) ;
#3577 = ORIENTED_EDGE('',*,*,#2770,.T.) ;
#3578 = ORIENTED_EDGE('',*,*,#2768,.T.) ;
#3579 = ORIENTED_EDGE('',*,*,#2756,.T.) ;
#3580 = ORIENTED_EDGE('',*,*,#2751,.T.) ;
#3581 = ORIENTED_EDGE('',*,*,#2760,.T.) ;
#3582 = ORIENTED_EDGE('',*,*,#2779,.F.) ;
#3583 = ORIENTED_EDGE('',*,*,#2780,.F.) ;
#3584 = ORIENTED_EDGE('',*,*,#2781,.F.) ;
#3585 = ORIENTED_EDGE('',*,*,#2759,.T.) ;
#3586 = ORIENTED_EDGE('',*,*,#2761,.T.) ;
#3587 = ORIENTED_EDGE('',*,*,#2782,.T.) ;
#3588 = ORIENTED_EDGE('',*,*,#2783,.F.) ;
#3589 = ORIENTED_EDGE('',*,*,#2784,.T.) ;
#3590 = ORIENTED_EDGE('',*,*,#2785,.T.) ;
#3591 = ORIENTED_EDGE('',*,*,#2779,.T.) ;
#3592 = ORIENTED_EDGE('',*,*,#2767,.T.) ;
#3593 = ORIENTED_EDGE('',*,*,#2786,.T.) ;
#3594 = ORIENTED_EDGE('',*,*,#2787,.F.) ;
#3595 = ORIENTED_EDGE('',*,*,#2782,.F.) ;
#3596 = ORIENTED_EDGE('',*,*,#2788,.T.) ;
#3597 = ORIENTED_EDGE('',*,*,#2789,.T.) ;
#3598 = ORIENTED_EDGE('',*,*,#2790,.T.) ;
#3599 = ORIENTED_EDGE('',*,*,#2791,.T.) ;
#3600 = ORIENTED_EDGE('',*,*,#2792,.T.) ;
#3601 = ORIENTED_EDGE('',*,*,#2793,.T.) ;
#3602 = ORIENTED_EDGE('',*,*,#2790,.F.) ;
#3603 = ORIENTED_EDGE('',*,*,#2794,.T.) ;
#3604 = ORIENTED_EDGE('',*,*,#2795,.T.) ;
#3605 = ORIENTED_EDGE('',*,*,#2796,.T.) ;
#3606 = ORIENTED_EDGE('',*,*,#2792,.F.) ;
#3607 = ORIENTED_EDGE('',*,*,#2797,.T.) ;
#3608 = ORIENTED_EDGE('',*,*,#2788,.F.) ;
#3609 = ORIENTED_EDGE('',*,*,#2798,.T.) ;
#3610 = ORIENTED_EDGE('',*,*,#2795,.F.) ;
#3611 = ORIENTED_EDGE('',*,*,#2799,.T.) ;
#3612 = ORIENTED_EDGE('',*,*,#2794,.F.) ;
#3613 = ORIENTED_EDGE('',*,*,#2800,.F.) ;
#3614 = ORIENTED_EDGE('',*,*,#2801,.T.) ;
#3615 = ORIENTED_EDGE('',*,*,#2802,.T.) ;
#3616 = ORIENTED_EDGE('',*,*,#2789,.F.) ;
#3617 = ORIENTED_EDGE('',*,*,#2803,.F.) ;
#3618 = ORIENTED_EDGE('',*,*,#2804,.T.) ;
#3619 = ORIENTED_EDGE('',*,*,#2800,.T.) ;
#3620 = ORIENTED_EDGE('',*,*,#2805,.F.) ;
#3621 = ORIENTED_EDGE('',*,*,#2806,.F.) ;
#3622 = ORIENTED_EDGE('',*,*,#2807,.F.) ;
#3623 = ORIENTED_EDGE('',*,*,#2808,.F.) ;
#3624 = ORIENTED_EDGE('',*,*,#2809,.F.) ;
#3625 = ORIENTED_EDGE('',*,*,#2810,.F.) ;
#3626 = ORIENTED_EDGE('',*,*,#2811,.F.) ;
#3627 = ORIENTED_EDGE('',*,*,#2791,.F.) ;
#3628 = ORIENTED_EDGE('',*,*,#2793,.F.) ;
#3629 = ORIENTED_EDGE('',*,*,#2796,.F.) ;
#3630 = ORIENTED_EDGE('',*,*,#2798,.F.) ;
#3631 = ORIENTED_EDGE('',*,*,#2811,.T.) ;
#3632 = ORIENTED_EDGE('',*,*,#2812,.T.) ;
#3633 = ORIENTED_EDGE('',*,*,#2813,.T.) ;
#3634 = ORIENTED_EDGE('',*,*,#2814,.T.) ;
#3635 = ORIENTED_EDGE('',*,*,#2812,.F.) ;
#3636 = ORIENTED_EDGE('',*,*,#2814,.F.) ;
#3637 = ORIENTED_EDGE('',*,*,#2815,.T.) ;
#3638 = ORIENTED_EDGE('',*,*,#2816,.T.) ;
#3639 = ORIENTED_EDGE('',*,*,#2815,.F.) ;
#3640 = ORIENTED_EDGE('',*,*,#2813,.F.) ;
#3641 = ORIENTED_EDGE('',*,*,#2817,.T.) ;
#3642 = ORIENTED_EDGE('',*,*,#2818,.T.) ;
#3643 = ORIENTED_EDGE('',*,*,#2819,.T.) ;
#3644 = ORIENTED_EDGE('',*,*,#2820,.T.) ;
#3645 = ORIENTED_EDGE('',*,*,#2818,.F.) ;
#3646 = ORIENTED_EDGE('',*,*,#2821,.F.) ;
#3647 = ORIENTED_EDGE('',*,*,#2822,.F.) ;
#3648 = ORIENTED_EDGE('',*,*,#2823,.F.) ;
#3649 = ORIENTED_EDGE('',*,*,#2824,.F.) ;
#3650 = ORIENTED_EDGE('',*,*,#2825,.F.) ;
#3651 = ORIENTED_EDGE('',*,*,#2826,.F.) ;
#3652 = ORIENTED_EDGE('',*,*,#2827,.F.) ;
#3653 = ORIENTED_EDGE('',*,*,#2828,.F.) ;
#3654 = ORIENTED_EDGE('',*,*,#2829,.F.) ;
#3655 = ORIENTED_EDGE('',*,*,#2830,.F.) ;
#3656 = ORIENTED_EDGE('',*,*,#2817,.F.) ;
#3657 = ORIENTED_EDGE('',*,*,#2820,.F.) ;
#3658 = ORIENTED_EDGE('',*,*,#2831,.T.) ;
#3659 = ORIENTED_EDGE('',*,*,#2832,.T.) ;
#3660 = ORIENTED_EDGE('',*,*,#2831,.F.) ;
#3661 = ORIENTED_EDGE('',*,*,#2819,.F.) ;
#3662 = ORIENTED_EDGE('',*,*,#2833,.T.) ;
#3663 = ORIENTED_EDGE('',*,*,#2834,.T.) ;
#3664 = ORIENTED_EDGE('',*,*,#2835,.T.) ;
#3665 = ORIENTED_EDGE('',*,*,#2827,.T.) ;
#3666 = ORIENTED_EDGE('',*,*,#2836,.T.) ;
#3667 = ORIENTED_EDGE('',*,*,#2828,.T.) ;
#3668 = ORIENTED_EDGE('',*,*,#2835,.F.) ;
#3669 = ORIENTED_EDGE('',*,*,#2837,.T.) ;
#3670 = ORIENTED_EDGE('',*,*,#2838,.T.) ;
#3671 = ORIENTED_EDGE('',*,*,#2829,.T.) ;
#3672 = ORIENTED_EDGE('',*,*,#2836,.F.) ;
#3673 = ORIENTED_EDGE('',*,*,#2839,.T.) ;
#3674 = ORIENTED_EDGE('',*,*,#2833,.F.) ;
#3675 = ORIENTED_EDGE('',*,*,#2830,.T.) ;
#3676 = ORIENTED_EDGE('',*,*,#2838,.F.) ;
#3677 = ORIENTED_EDGE('',*,*,#2840,.T.) ;
#3678 = ORIENTED_EDGE('',*,*,#2837,.F.) ;
#3679 = ORIENTED_EDGE('',*,*,#2841,.F.) ;
#3680 = ORIENTED_EDGE('',*,*,#2842,.T.) ;
#3681 = ORIENTED_EDGE('',*,*,#2843,.T.) ;
#3682 = ORIENTED_EDGE('',*,*,#2834,.F.) ;
#3683 = ORIENTED_EDGE('',*,*,#2844,.F.) ;
#3684 = ORIENTED_EDGE('',*,*,#2845,.T.) ;
#3685 = ORIENTED_EDGE('',*,*,#2841,.T.) ;
#3686 = ORIENTED_EDGE('',*,*,#2787,.T.) ;
#3687 = ORIENTED_EDGE('',*,*,#2846,.T.) ;
#3688 = ORIENTED_EDGE('',*,*,#2847,.T.) ;
#3689 = ORIENTED_EDGE('',*,*,#2783,.T.) ;
#3690 = ORIENTED_EDGE('',*,*,#2848,.T.) ;
#3691 = ORIENTED_EDGE('',*,*,#2849,.T.) ;
#3692 = ORIENTED_EDGE('',*,*,#2847,.F.) ;
#3693 = ORIENTED_EDGE('',*,*,#2850,.T.) ;
#3694 = ORIENTED_EDGE('',*,*,#2851,.T.) ;
#3695 = ORIENTED_EDGE('',*,*,#2852,.T.) ;
#3696 = ORIENTED_EDGE('',*,*,#2853,.T.) ;
#3697 = ORIENTED_EDGE('',*,*,#2821,.T.) ;
#3698 = ORIENTED_EDGE('',*,*,#2851,.F.) ;
#3699 = ORIENTED_EDGE('',*,*,#2854,.T.) ;
#3700 = ORIENTED_EDGE('',*,*,#2848,.F.) ;
#3701 = ORIENTED_EDGE('',*,*,#2855,.T.) ;
#3702 = ORIENTED_EDGE('',*,*,#2856,.T.) ;
#3703 = ORIENTED_EDGE('',*,*,#2857,.T.) ;
#3704 = ORIENTED_EDGE('',*,*,#2823,.T.) ;
#3705 = ORIENTED_EDGE('',*,*,#2858,.T.) ;
#3706 = ORIENTED_EDGE('',*,*,#2859,.T.) ;
#3707 = ORIENTED_EDGE('',*,*,#2807,.T.) ;
#3708 = ORIENTED_EDGE('',*,*,#2860,.T.) ;
#3709 = ORIENTED_EDGE('',*,*,#2861,.T.) ;
#3710 = ORIENTED_EDGE('',*,*,#2806,.T.) ;
#3711 = ORIENTED_EDGE('',*,*,#2862,.T.) ;
#3712 = ORIENTED_EDGE('',*,*,#2863,.T.) ;
#3713 = ORIENTED_EDGE('',*,*,#2860,.F.) ;
#3714 = ORIENTED_EDGE('',*,*,#2864,.T.) ;
#3715 = ORIENTED_EDGE('',*,*,#2865,.T.) ;
#3716 = ORIENTED_EDGE('',*,*,#2866,.T.) ;
#3717 = ORIENTED_EDGE('',*,*,#2867,.T.) ;
#3718 = ORIENTED_EDGE('',*,*,#2868,.T.) ;
#3719 = ORIENTED_EDGE('',*,*,#2869,.T.) ;
#3720 = ORIENTED_EDGE('',*,*,#2870,.T.) ;
#3721 = ORIENTED_EDGE('',*,*,#2871,.T.) ;
#3722 = ORIENTED_EDGE('',*,*,#2872,.T.) ;
#3723 = ORIENTED_EDGE('',*,*,#2873,.T.) ;
#3724 = ORIENTED_EDGE('',*,*,#2874,.T.) ;
#3725 = ORIENTED_EDGE('',*,*,#2870,.F.) ;
#3726 = ORIENTED_EDGE('',*,*,#2875,.T.) ;
#3727 = ORIENTED_EDGE('',*,*,#2876,.T.) ;
#3728 = ORIENTED_EDGE('',*,*,#2873,.F.) ;
#3729 = ORIENTED_EDGE('',*,*,#2877,.T.) ;
#3730 = ORIENTED_EDGE('',*,*,#2867,.F.) ;
#3731 = ORIENTED_EDGE('',*,*,#2805,.T.) ;
#3732 = ORIENTED_EDGE('',*,*,#2878,.T.) ;
#3733 = ORIENTED_EDGE('',*,*,#2879,.T.) ;
#3734 = ORIENTED_EDGE('',*,*,#2862,.F.) ;
#3735 = ORIENTED_EDGE('',*,*,#2880,.T.) ;
#3736 = ORIENTED_EDGE('',*,*,#2878,.F.) ;
#3737 = ORIENTED_EDGE('',*,*,#2881,.T.) ;
#3738 = ORIENTED_EDGE('',*,*,#2882,.T.) ;
#3739 = ORIENTED_EDGE('',*,*,#2872,.F.) ;
#3740 = ORIENTED_EDGE('',*,*,#2883,.T.) ;
#3741 = ORIENTED_EDGE('',*,*,#2865,.F.) ;
#3742 = ORIENTED_EDGE('',*,*,#2825,.T.) ;
#3743 = ORIENTED_EDGE('',*,*,#2884,.T.) ;
#3744 = ORIENTED_EDGE('',*,*,#2857,.F.) ;
#3745 = ORIENTED_EDGE('',*,*,#2885,.T.) ;
#3746 = ORIENTED_EDGE('',*,*,#2884,.F.) ;
#3747 = ORIENTED_EDGE('',*,*,#2824,.T.) ;
#3748 = ORIENTED_EDGE('',*,*,#2859,.F.) ;
#3749 = ORIENTED_EDGE('',*,*,#2886,.T.) ;
#3750 = ORIENTED_EDGE('',*,*,#2887,.T.) ;
#3751 = ORIENTED_EDGE('',*,*,#2808,.T.) ;
#3752 = ORIENTED_EDGE('',*,*,#2822,.T.) ;
#3753 = ORIENTED_EDGE('',*,*,#2888,.T.) ;
#3754 = ORIENTED_EDGE('',*,*,#2889,.T.) ;
#3755 = ORIENTED_EDGE('',*,*,#2858,.F.) ;
#3756 = ORIENTED_EDGE('',*,*,#2890,.T.) ;
#3757 = ORIENTED_EDGE('',*,*,#2891,.T.) ;
#3758 = ORIENTED_EDGE('',*,*,#2892,.T.) ;
#3759 = ORIENTED_EDGE('',*,*,#2809,.T.) ;
#3760 = ORIENTED_EDGE('',*,*,#2893,.T.) ;
#3761 = ORIENTED_EDGE('',*,*,#2894,.T.) ;
#3762 = ORIENTED_EDGE('',*,*,#2892,.F.) ;
#3763 = ORIENTED_EDGE('',*,*,#2895,.T.) ;
#3764 = ORIENTED_EDGE('',*,*,#2896,.T.) ;
#3765 = ORIENTED_EDGE('',*,*,#2897,.T.) ;
#3766 = ORIENTED_EDGE('',*,*,#2893,.F.) ;
#3767 = ORIENTED_EDGE('',*,*,#2898,.T.) ;
#3768 = ORIENTED_EDGE('',*,*,#2899,.T.) ;
#3769 = ORIENTED_EDGE('',*,*,#2900,.T.) ;
#3770 = ORIENTED_EDGE('',*,*,#2896,.F.) ;
#3771 = ORIENTED_EDGE('',*,*,#2901,.T.) ;
#3772 = ORIENTED_EDGE('',*,*,#2890,.F.) ;
#3773 = ORIENTED_EDGE('',*,*,#2887,.F.) ;
#3774 = ORIENTED_EDGE('',*,*,#2902,.T.) ;
#3775 = ORIENTED_EDGE('',*,*,#2888,.F.) ;
#3776 = ORIENTED_EDGE('',*,*,#2853,.F.) ;
#3777 = ORIENTED_EDGE('',*,*,#2903,.T.) ;
#3778 = ORIENTED_EDGE('',*,*,#2849,.F.) ;
#3779 = ORIENTED_EDGE('',*,*,#2904,.F.) ;
#3780 = ORIENTED_EDGE('',*,*,#2905,.T.) ;
#3781 = ORIENTED_EDGE('',*,*,#2906,.F.) ;
#3782 = ORIENTED_EDGE('',*,*,#2907,.F.) ;
#3783 = ORIENTED_EDGE('',*,*,#2908,.F.) ;
#3784 = ORIENTED_EDGE('',*,*,#2784,.F.) ;
#3785 = ORIENTED_EDGE('',*,*,#2754,.T.) ;
#3786 = ORIENTED_EDGE('',*,*,#2854,.F.) ;
#3787 = ORIENTED_EDGE('',*,*,#2826,.T.) ;
#3788 = ORIENTED_EDGE('',*,*,#2864,.F.) ;
#3789 = ORIENTED_EDGE('',*,*,#2909,.F.) ;
#3790 = ORIENTED_EDGE('',*,*,#2904,.T.) ;
#3791 = ORIENTED_EDGE('',*,*,#2875,.F.) ;
#3792 = ORIENTED_EDGE('',*,*,#2910,.F.) ;
#3793 = ORIENTED_EDGE('',*,*,#2868,.F.) ;
#3794 = ORIENTED_EDGE('',*,*,#2877,.F.) ;
#3795 = ORIENTED_EDGE('',*,*,#2910,.T.) ;
#3796 = ORIENTED_EDGE('',*,*,#2869,.F.) ;
#3797 = ORIENTED_EDGE('',*,*,#2882,.F.) ;
#3798 = ORIENTED_EDGE('',*,*,#2911,.T.) ;
#3799 = ORIENTED_EDGE('',*,*,#2912,.T.) ;
#3800 = ORIENTED_EDGE('',*,*,#2909,.T.) ;
#3801 = ORIENTED_EDGE('',*,*,#2881,.F.) ;
#3802 = ORIENTED_EDGE('',*,*,#2810,.T.) ;
#3803 = ORIENTED_EDGE('',*,*,#2894,.F.) ;
#3804 = ORIENTED_EDGE('',*,*,#2913,.T.) ;
#3805 = ORIENTED_EDGE('',*,*,#2911,.F.) ;
#3806 = ORIENTED_EDGE('',*,*,#2897,.F.) ;
#3807 = ORIENTED_EDGE('',*,*,#2914,.F.) ;
#3808 = ORIENTED_EDGE('',*,*,#2915,.F.) ;
#3809 = ORIENTED_EDGE('',*,*,#2916,.F.) ;
#3810 = ORIENTED_EDGE('',*,*,#2917,.F.) ;
#3811 = ORIENTED_EDGE('',*,*,#2918,.F.) ;
#3812 = ORIENTED_EDGE('',*,*,#2913,.F.) ;
#3813 = ORIENTED_EDGE('',*,*,#2749,.T.) ;
#3814 = ORIENTED_EDGE('',*,*,#2755,.T.) ;
#3815 = ORIENTED_EDGE('',*,*,#2781,.T.) ;
#3816 = ORIENTED_EDGE('',*,*,#2919,.F.) ;
#3817 = ORIENTED_EDGE('',*,*,#2914,.T.) ;
#3818 = ORIENTED_EDGE('',*,*,#2900,.F.) ;
#3819 = ORIENTED_EDGE('',*,*,#2920,.T.) ;
#3820 = ORIENTED_EDGE('',*,*,#2776,.T.) ;
#3821 = ORIENTED_EDGE('',*,*,#2921,.T.) ;
#3822 = ORIENTED_EDGE('',*,*,#2922,.T.) ;
#3823 = ORIENTED_EDGE('',*,*,#2907,.T.) ;
#3824 = ORIENTED_EDGE('',*,*,#2923,.T.) ;
#3825 = ORIENTED_EDGE('',*,*,#2922,.F.) ;
#3826 = ORIENTED_EDGE('',*,*,#2924,.T.) ;
#3827 = ORIENTED_EDGE('',*,*,#2785,.F.) ;
#3828 = ORIENTED_EDGE('',*,*,#2908,.T.) ;
#3829 = ORIENTED_EDGE('',*,*,#2906,.T.) ;
#3830 = ORIENTED_EDGE('',*,*,#2925,.T.) ;
#3831 = ORIENTED_EDGE('',*,*,#2926,.T.) ;
#3832 = ORIENTED_EDGE('',*,*,#2927,.T.) ;
#3833 = ORIENTED_EDGE('',*,*,#2923,.F.) ;
#3834 = ORIENTED_EDGE('',*,*,#2777,.T.) ;
#3835 = ORIENTED_EDGE('',*,*,#2920,.F.) ;
#3836 = ORIENTED_EDGE('',*,*,#2899,.F.) ;
#3837 = ORIENTED_EDGE('',*,*,#2928,.T.) ;
#3838 = ORIENTED_EDGE('',*,*,#2924,.F.) ;
#3839 = ORIENTED_EDGE('',*,*,#2929,.F.) ;
#3840 = ORIENTED_EDGE('',*,*,#2930,.F.) ;
#3841 = ORIENTED_EDGE('',*,*,#2780,.T.) ;
#3842 = ORIENTED_EDGE('',*,*,#2921,.F.) ;
#3843 = ORIENTED_EDGE('',*,*,#2931,.F.) ;
#3844 = ORIENTED_EDGE('',*,*,#2932,.F.) ;
#3845 = ORIENTED_EDGE('',*,*,#2929,.T.) ;
#3846 = ORIENTED_EDGE('',*,*,#2927,.F.) ;
#3847 = ORIENTED_EDGE('',*,*,#2933,.F.) ;
#3848 = ORIENTED_EDGE('',*,*,#2934,.F.) ;
#3849 = ORIENTED_EDGE('',*,*,#2931,.T.) ;
#3850 = ORIENTED_EDGE('',*,*,#2926,.F.) ;
#3851 = ORIENTED_EDGE('',*,*,#2935,.F.) ;
#3852 = ORIENTED_EDGE('',*,*,#2936,.F.) ;
#3853 = ORIENTED_EDGE('',*,*,#2933,.T.) ;
#3854 = ORIENTED_EDGE('',*,*,#2934,.T.) ;
#3855 = ORIENTED_EDGE('',*,*,#2936,.T.) ;
#3856 = ORIENTED_EDGE('',*,*,#2937,.T.) ;
#3857 = ORIENTED_EDGE('',*,*,#2917,.T.) ;
#3858 = ORIENTED_EDGE('',*,*,#2938,.T.) ;
#3859 = ORIENTED_EDGE('',*,*,#2939,.T.) ;
#3860 = ORIENTED_EDGE('',*,*,#2915,.T.) ;
#3861 = ORIENTED_EDGE('',*,*,#2919,.T.) ;
#3862 = ORIENTED_EDGE('',*,*,#2930,.T.) ;
#3863 = ORIENTED_EDGE('',*,*,#2916,.T.) ;
#3864 = ORIENTED_EDGE('',*,*,#2939,.F.) ;
#3865 = ORIENTED_EDGE('',*,*,#2932,.T.) ;
#3866 = ORIENTED_EDGE('',*,*,#2938,.F.) ;
#3867 = ORIENTED_EDGE('',*,*,#2912,.F.) ;
#3868 = ORIENTED_EDGE('',*,*,#2918,.T.) ;
#3869 = ORIENTED_EDGE('',*,*,#2937,.F.) ;
#3870 = ORIENTED_EDGE('',*,*,#2935,.T.) ;
#3871 = ORIENTED_EDGE('',*,*,#2925,.F.) ;
#3872 = ORIENTED_EDGE('',*,*,#2905,.F.) ;
#3873 = ORIENTED_EDGE('',*,*,#2746,.T.) ;
#3874 = ORIENTED_EDGE('',*,*,#2799,.F.) ;
#3875 = ORIENTED_EDGE('',*,*,#2940,.F.) ;
#3876 = ORIENTED_EDGE('',*,*,#2941,.T.) ;
#3877 = ORIENTED_EDGE('',*,*,#2803,.T.) ;
#3878 = ORIENTED_EDGE('',*,*,#2797,.F.) ;
#3879 = ORIENTED_EDGE('',*,*,#2802,.F.) ;
#3880 = ORIENTED_EDGE('',*,*,#2942,.T.) ;
#3881 = ORIENTED_EDGE('',*,*,#2940,.T.) ;
#3882 = ORIENTED_EDGE('',*,*,#2840,.F.) ;
#3883 = ORIENTED_EDGE('',*,*,#2943,.F.) ;
#3884 = ORIENTED_EDGE('',*,*,#2944,.T.) ;
#3885 = ORIENTED_EDGE('',*,*,#2844,.T.) ;
#3886 = ORIENTED_EDGE('',*,*,#2839,.F.) ;
#3887 = ORIENTED_EDGE('',*,*,#2843,.F.) ;
#3888 = ORIENTED_EDGE('',*,*,#2945,.T.) ;
#3889 = ORIENTED_EDGE('',*,*,#2943,.T.) ;
#3890 = ORIENTED_EDGE('',*,*,#2886,.F.) ;
#3891 = ORIENTED_EDGE('',*,*,#2946,.F.) ;
#3892 = ORIENTED_EDGE('',*,*,#2947,.F.) ;
#3893 = ORIENTED_EDGE('',*,*,#2948,.T.) ;
#3894 = ORIENTED_EDGE('',*,*,#2861,.F.) ;
#3895 = ORIENTED_EDGE('',*,*,#2949,.F.) ;
#3896 = ORIENTED_EDGE('',*,*,#2950,.T.) ;
#3897 = ORIENTED_EDGE('',*,*,#2946,.T.) ;
#3898 = ORIENTED_EDGE('',*,*,#2863,.F.) ;
#3899 = ORIENTED_EDGE('',*,*,#2951,.F.) ;
#3900 = ORIENTED_EDGE('',*,*,#2952,.F.) ;
#3901 = ORIENTED_EDGE('',*,*,#2949,.T.) ;
#3902 = ORIENTED_EDGE('',*,*,#2883,.F.) ;
#3903 = ORIENTED_EDGE('',*,*,#2953,.F.) ;
#3904 = ORIENTED_EDGE('',*,*,#2954,.T.) ;
#3905 = ORIENTED_EDGE('',*,*,#2951,.T.) ;
#3906 = ORIENTED_EDGE('',*,*,#2879,.F.) ;
#3907 = ORIENTED_EDGE('',*,*,#2880,.F.) ;
#3908 = ORIENTED_EDGE('',*,*,#2871,.F.) ;
#3909 = ORIENTED_EDGE('',*,*,#2874,.F.) ;
#3910 = ORIENTED_EDGE('',*,*,#2876,.F.) ;
#3911 = ORIENTED_EDGE('',*,*,#2866,.F.) ;
#3912 = ORIENTED_EDGE('',*,*,#2885,.F.) ;
#3913 = ORIENTED_EDGE('',*,*,#2955,.F.) ;
#3914 = ORIENTED_EDGE('',*,*,#2956,.F.) ;
#3915 = ORIENTED_EDGE('',*,*,#2953,.T.) ;
#3916 = ORIENTED_EDGE('',*,*,#2856,.F.) ;
#3917 = ORIENTED_EDGE('',*,*,#2957,.F.) ;
#3918 = ORIENTED_EDGE('',*,*,#2958,.T.) ;
#3919 = ORIENTED_EDGE('',*,*,#2955,.T.) ;
#3920 = ORIENTED_EDGE('',*,*,#2889,.F.) ;
#3921 = ORIENTED_EDGE('',*,*,#2959,.F.) ;
#3922 = ORIENTED_EDGE('',*,*,#2960,.F.) ;
#3923 = ORIENTED_EDGE('',*,*,#2957,.T.) ;
#3924 = ORIENTED_EDGE('',*,*,#2903,.F.) ;
#3925 = ORIENTED_EDGE('',*,*,#2961,.F.) ;
#3926 = ORIENTED_EDGE('',*,*,#2962,.T.) ;
#3927 = ORIENTED_EDGE('',*,*,#2959,.T.) ;
#3928 = ORIENTED_EDGE('',*,*,#2778,.T.) ;
#3929 = ORIENTED_EDGE('',*,*,#2928,.F.) ;
#3930 = ORIENTED_EDGE('',*,*,#2901,.F.) ;
#3931 = ORIENTED_EDGE('',*,*,#2898,.F.) ;
#3932 = ORIENTED_EDGE('',*,*,#2895,.F.) ;
#3933 = ORIENTED_EDGE('',*,*,#2891,.F.) ;
#3934 = ORIENTED_EDGE('',*,*,#2963,.F.) ;
#3935 = ORIENTED_EDGE('',*,*,#2964,.F.) ;
#3936 = ORIENTED_EDGE('',*,*,#2961,.T.) ;
#3937 = ORIENTED_EDGE('',*,*,#2852,.F.) ;
#3938 = ORIENTED_EDGE('',*,*,#2855,.F.) ;
#3939 = ORIENTED_EDGE('',*,*,#2850,.F.) ;
#3940 = ORIENTED_EDGE('',*,*,#2846,.F.) ;
#3941 = ORIENTED_EDGE('',*,*,#2786,.F.) ;
#3942 = ORIENTED_EDGE('',*,*,#2766,.T.) ;
#3943 = ORIENTED_EDGE('',*,*,#2774,.T.) ;
#3944 = ORIENTED_EDGE('',*,*,#2902,.F.) ;
#3945 = ORIENTED_EDGE('',*,*,#2948,.F.) ;
#3946 = ORIENTED_EDGE('',*,*,#2965,.T.) ;
#3947 = ORIENTED_EDGE('',*,*,#2963,.T.) ;
#3948 = ORIENTED_EDGE('',*,*,#2965,.F.) ;
#3949 = ORIENTED_EDGE('',*,*,#2947,.T.) ;
#3950 = ORIENTED_EDGE('',*,*,#2950,.F.) ;
#3951 = ORIENTED_EDGE('',*,*,#2952,.T.) ;
#3952 = ORIENTED_EDGE('',*,*,#2954,.F.) ;
#3953 = ORIENTED_EDGE('',*,*,#2956,.T.) ;
#3954 = ORIENTED_EDGE('',*,*,#2958,.F.) ;
#3955 = ORIENTED_EDGE('',*,*,#2960,.T.) ;
#3956 = ORIENTED_EDGE('',*,*,#2962,.F.) ;
#3957 = ORIENTED_EDGE('',*,*,#2964,.T.) ;
#3958 = ORIENTED_EDGE('',*,*,#2832,.F.) ;
#3959 = ORIENTED_EDGE('',*,*,#2845,.F.) ;
#3960 = ORIENTED_EDGE('',*,*,#2944,.F.) ;
#3961 = ORIENTED_EDGE('',*,*,#2945,.F.) ;
#3962 = ORIENTED_EDGE('',*,*,#2842,.F.) ;
#3963 = ORIENTED_EDGE('',*,*,#2816,.F.) ;
#3964 = ORIENTED_EDGE('',*,*,#2804,.F.) ;
#3965 = ORIENTED_EDGE('',*,*,#2941,.F.) ;
#3966 = ORIENTED_EDGE('',*,*,#2942,.F.) ;
#3967 = ORIENTED_EDGE('',*,*,#2801,.F.) ;
#3968 = ORIENTED_EDGE('',*,*,#2966,.T.) ;
#3969 = ORIENTED_EDGE('',*,*,#2967,.T.) ;
#3970 = ORIENTED_EDGE('',*,*,#2968,.T.) ;
#3971 = ORIENTED_EDGE('',*,*,#2969,.T.) ;
#3972 = ORIENTED_EDGE('',*,*,#2970,.T.) ;
#3973 = ORIENTED_EDGE('',*,*,#2971,.T.) ;
#3974 = ORIENTED_EDGE('',*,*,#2972,.T.) ;
#3975 = ORIENTED_EDGE('',*,*,#2968,.F.) ;
#3976 = ORIENTED_EDGE('',*,*,#2973,.T.) ;
#3977 = ORIENTED_EDGE('',*,*,#2973,.F.) ;
#3978 = ORIENTED_EDGE('',*,*,#2967,.F.) ;
#3979 = ORIENTED_EDGE('',*,*,#2974,.T.) ;
#3980 = ORIENTED_EDGE('',*,*,#2975,.F.) ;
#3981 = ORIENTED_EDGE('',*,*,#2976,.F.) ;
#3982 = ORIENTED_EDGE('',*,*,#2977,.F.) ;
#3983 = ORIENTED_EDGE('',*,*,#2978,.T.) ;
#3984 = ORIENTED_EDGE('',*,*,#2979,.T.) ;
#3985 = ORIENTED_EDGE('',*,*,#2980,.T.) ;
#3986 = ORIENTED_EDGE('',*,*,#2981,.T.) ;
#3987 = ORIENTED_EDGE('',*,*,#2982,.T.) ;
#3988 = ORIENTED_EDGE('',*,*,#2983,.F.) ;
#3989 = ORIENTED_EDGE('',*,*,#2984,.T.) ;
#3990 = ORIENTED_EDGE('',*,*,#2979,.F.) ;
#3991 = ORIENTED_EDGE('',*,*,#2985,.T.) ;
#3992 = ORIENTED_EDGE('',*,*,#2986,.F.) ;
#3993 = ORIENTED_EDGE('',*,*,#2985,.F.) ;
#3994 = ORIENTED_EDGE('',*,*,#2982,.F.) ;
#3995 = ORIENTED_EDGE('',*,*,#2987,.T.) ;
#3996 = ORIENTED_EDGE('',*,*,#2988,.T.) ;
#3997 = ORIENTED_EDGE('',*,*,#2989,.T.) ;
#3998 = ORIENTED_EDGE('',*,*,#2990,.T.) ;
#3999 = ORIENTED_EDGE('',*,*,#2991,.T.) ;
#4000 = ORIENTED_EDGE('',*,*,#2992,.T.) ;
#4001 = ORIENTED_EDGE('',*,*,#2993,.T.) ;
#4002 = ORIENTED_EDGE('',*,*,#2994,.T.) ;
#4003 = ORIENTED_EDGE('',*,*,#2995,.T.) ;
#4004 = ORIENTED_EDGE('',*,*,#2996,.T.) ;
#4005 = ORIENTED_EDGE('',*,*,#2997,.T.) ;
#4006 = ORIENTED_EDGE('',*,*,#2994,.F.) ;
#4007 = ORIENTED_EDGE('',*,*,#2998,.T.) ;
#4008 = ORIENTED_EDGE('',*,*,#2999,.T.) ;
#4009 = ORIENTED_EDGE('',*,*,#3000,.T.) ;
#4010 = ORIENTED_EDGE('',*,*,#2996,.F.) ;
#4011 = ORIENTED_EDGE('',*,*,#3001,.T.) ;
#4012 = ORIENTED_EDGE('',*,*,#2992,.F.) ;
#4013 = ORIENTED_EDGE('',*,*,#3002,.T.) ;
#4014 = ORIENTED_EDGE('',*,*,#2999,.F.) ;
#4015 = ORIENTED_EDGE('',*,*,#3003,.T.) ;
#4016 = ORIENTED_EDGE('',*,*,#2998,.F.) ;
#4017 = ORIENTED_EDGE('',*,*,#3004,.F.) ;
#4018 = ORIENTED_EDGE('',*,*,#3005,.T.) ;
#4019 = ORIENTED_EDGE('',*,*,#3006,.T.) ;
#4020 = ORIENTED_EDGE('',*,*,#2993,.F.) ;
#4021 = ORIENTED_EDGE('',*,*,#3007,.F.) ;
#4022 = ORIENTED_EDGE('',*,*,#3008,.T.) ;
#4023 = ORIENTED_EDGE('',*,*,#3004,.T.) ;
#4024 = ORIENTED_EDGE('',*,*,#2969,.F.) ;
#4025 = ORIENTED_EDGE('',*,*,#3009,.F.) ;
#4026 = ORIENTED_EDGE('',*,*,#3010,.F.) ;
#4027 = ORIENTED_EDGE('',*,*,#3011,.F.) ;
#4028 = ORIENTED_EDGE('',*,*,#3012,.F.) ;
#4029 = ORIENTED_EDGE('',*,*,#3013,.F.) ;
#4030 = ORIENTED_EDGE('',*,*,#3014,.F.) ;
#4031 = ORIENTED_EDGE('',*,*,#3015,.F.) ;
#4032 = ORIENTED_EDGE('',*,*,#3016,.F.) ;
#4033 = ORIENTED_EDGE('',*,*,#3017,.F.) ;
#4034 = ORIENTED_EDGE('',*,*,#2984,.F.) ;
#4035 = ORIENTED_EDGE('',*,*,#3018,.F.) ;
#4036 = ORIENTED_EDGE('',*,*,#3019,.F.) ;
#4037 = ORIENTED_EDGE('',*,*,#3020,.F.) ;
#4038 = ORIENTED_EDGE('',*,*,#3021,.F.) ;
#4039 = ORIENTED_EDGE('',*,*,#3022,.F.) ;
#4040 = ORIENTED_EDGE('',*,*,#2995,.F.) ;
#4041 = ORIENTED_EDGE('',*,*,#2997,.F.) ;
#4042 = ORIENTED_EDGE('',*,*,#3000,.F.) ;
#4043 = ORIENTED_EDGE('',*,*,#3002,.F.) ;
#4044 = ORIENTED_EDGE('',*,*,#3023,.T.) ;
#4045 = ORIENTED_EDGE('',*,*,#3024,.T.) ;
#4046 = ORIENTED_EDGE('',*,*,#3025,.T.) ;
#4047 = ORIENTED_EDGE('',*,*,#3019,.T.) ;
#4048 = ORIENTED_EDGE('',*,*,#3026,.T.) ;
#4049 = ORIENTED_EDGE('',*,*,#3020,.T.) ;
#4050 = ORIENTED_EDGE('',*,*,#3025,.F.) ;
#4051 = ORIENTED_EDGE('',*,*,#3027,.T.) ;
#4052 = ORIENTED_EDGE('',*,*,#3028,.T.) ;
#4053 = ORIENTED_EDGE('',*,*,#3021,.T.) ;
#4054 = ORIENTED_EDGE('',*,*,#3026,.F.) ;
#4055 = ORIENTED_EDGE('',*,*,#3029,.T.) ;
#4056 = ORIENTED_EDGE('',*,*,#3023,.F.) ;
#4057 = ORIENTED_EDGE('',*,*,#3022,.T.) ;
#4058 = ORIENTED_EDGE('',*,*,#3028,.F.) ;
#4059 = ORIENTED_EDGE('',*,*,#3030,.T.) ;
#4060 = ORIENTED_EDGE('',*,*,#3027,.F.) ;
#4061 = ORIENTED_EDGE('',*,*,#3031,.F.) ;
#4062 = ORIENTED_EDGE('',*,*,#3032,.T.) ;
#4063 = ORIENTED_EDGE('',*,*,#3033,.T.) ;
#4064 = ORIENTED_EDGE('',*,*,#3024,.F.) ;
#4065 = ORIENTED_EDGE('',*,*,#3034,.F.) ;
#4066 = ORIENTED_EDGE('',*,*,#3035,.T.) ;
#4067 = ORIENTED_EDGE('',*,*,#3031,.T.) ;
#4068 = ORIENTED_EDGE('',*,*,#3036,.T.) ;
#4069 = ORIENTED_EDGE('',*,*,#2970,.F.) ;
#4070 = ORIENTED_EDGE('',*,*,#3018,.T.) ;
#4071 = ORIENTED_EDGE('',*,*,#2983,.T.) ;
#4072 = ORIENTED_EDGE('',*,*,#3036,.F.) ;
#4073 = ORIENTED_EDGE('',*,*,#2986,.T.) ;
#4074 = ORIENTED_EDGE('',*,*,#2990,.F.) ;
#4075 = ORIENTED_EDGE('',*,*,#3037,.F.) ;
#4076 = ORIENTED_EDGE('',*,*,#2974,.F.) ;
#4077 = ORIENTED_EDGE('',*,*,#2966,.F.) ;
#4078 = ORIENTED_EDGE('',*,*,#3038,.T.) ;
#4079 = ORIENTED_EDGE('',*,*,#3039,.T.) ;
#4080 = ORIENTED_EDGE('',*,*,#3014,.T.) ;
#4081 = ORIENTED_EDGE('',*,*,#3040,.T.) ;
#4082 = ORIENTED_EDGE('',*,*,#3039,.F.) ;
#4083 = ORIENTED_EDGE('',*,*,#3041,.T.) ;
#4084 = ORIENTED_EDGE('',*,*,#3042,.T.) ;
#4085 = ORIENTED_EDGE('',*,*,#3015,.T.) ;
#4086 = ORIENTED_EDGE('',*,*,#3043,.T.) ;
#4087 = ORIENTED_EDGE('',*,*,#3016,.T.) ;
#4088 = ORIENTED_EDGE('',*,*,#3042,.F.) ;
#4089 = ORIENTED_EDGE('',*,*,#3044,.T.) ;
#4090 = ORIENTED_EDGE('',*,*,#2980,.F.) ;
#4091 = ORIENTED_EDGE('',*,*,#3017,.T.) ;
#4092 = ORIENTED_EDGE('',*,*,#3043,.F.) ;
#4093 = ORIENTED_EDGE('',*,*,#3045,.T.) ;
#4094 = ORIENTED_EDGE('',*,*,#3046,.T.) ;
#4095 = ORIENTED_EDGE('',*,*,#3047,.T.) ;
#4096 = ORIENTED_EDGE('',*,*,#3012,.T.) ;
#4097 = ORIENTED_EDGE('',*,*,#3048,.T.) ;
#4098 = ORIENTED_EDGE('',*,*,#3013,.T.) ;
#4099 = ORIENTED_EDGE('',*,*,#3047,.F.) ;
#4100 = ORIENTED_EDGE('',*,*,#3049,.T.) ;
#4101 = ORIENTED_EDGE('',*,*,#3040,.F.) ;
#4102 = ORIENTED_EDGE('',*,*,#2972,.F.) ;
#4103 = ORIENTED_EDGE('',*,*,#3050,.T.) ;
#4104 = ORIENTED_EDGE('',*,*,#3051,.T.) ;
#4105 = ORIENTED_EDGE('',*,*,#3009,.T.) ;
#4106 = ORIENTED_EDGE('',*,*,#3052,.T.) ;
#4107 = ORIENTED_EDGE('',*,*,#3010,.T.) ;
#4108 = ORIENTED_EDGE('',*,*,#3051,.F.) ;
#4109 = ORIENTED_EDGE('',*,*,#3053,.T.) ;
#4110 = ORIENTED_EDGE('',*,*,#3011,.T.) ;
#4111 = ORIENTED_EDGE('',*,*,#3052,.F.) ;
#4112 = ORIENTED_EDGE('',*,*,#3054,.T.) ;
#4113 = ORIENTED_EDGE('',*,*,#3048,.F.) ;
#4114 = ORIENTED_EDGE('',*,*,#2981,.F.) ;
#4115 = ORIENTED_EDGE('',*,*,#3045,.F.) ;
#4116 = ORIENTED_EDGE('',*,*,#3055,.F.) ;
#4117 = ORIENTED_EDGE('',*,*,#3056,.F.) ;
#4118 = ORIENTED_EDGE('',*,*,#3057,.T.) ;
#4119 = ORIENTED_EDGE('',*,*,#3058,.T.) ;
#4120 = ORIENTED_EDGE('',*,*,#2987,.F.) ;
#4121 = ORIENTED_EDGE('',*,*,#3044,.F.) ;
#4122 = ORIENTED_EDGE('',*,*,#3059,.F.) ;
#4123 = ORIENTED_EDGE('',*,*,#3060,.T.) ;
#4124 = ORIENTED_EDGE('',*,*,#3055,.T.) ;
#4125 = ORIENTED_EDGE('',*,*,#3041,.F.) ;
#4126 = ORIENTED_EDGE('',*,*,#3061,.F.) ;
#4127 = ORIENTED_EDGE('',*,*,#3062,.F.) ;
#4128 = ORIENTED_EDGE('',*,*,#3059,.T.) ;
#4129 = ORIENTED_EDGE('',*,*,#3038,.F.) ;
#4130 = ORIENTED_EDGE('',*,*,#3063,.F.) ;
#4131 = ORIENTED_EDGE('',*,*,#3064,.T.) ;
#4132 = ORIENTED_EDGE('',*,*,#3061,.T.) ;
#4133 = ORIENTED_EDGE('',*,*,#3049,.F.) ;
#4134 = ORIENTED_EDGE('',*,*,#3065,.F.) ;
#4135 = ORIENTED_EDGE('',*,*,#3066,.T.) ;
#4136 = ORIENTED_EDGE('',*,*,#3063,.T.) ;
#4137 = ORIENTED_EDGE('',*,*,#3046,.F.) ;
#4138 = ORIENTED_EDGE('',*,*,#3067,.F.) ;
#4139 = ORIENTED_EDGE('',*,*,#3068,.T.) ;
#4140 = ORIENTED_EDGE('',*,*,#3065,.T.) ;
#4141 = ORIENTED_EDGE('',*,*,#3054,.F.) ;
#4142 = ORIENTED_EDGE('',*,*,#3069,.F.) ;
#4143 = ORIENTED_EDGE('',*,*,#3070,.F.) ;
#4144 = ORIENTED_EDGE('',*,*,#3067,.T.) ;
#4145 = ORIENTED_EDGE('',*,*,#3053,.F.) ;
#4146 = ORIENTED_EDGE('',*,*,#3071,.F.) ;
#4147 = ORIENTED_EDGE('',*,*,#3072,.T.) ;
#4148 = ORIENTED_EDGE('',*,*,#3069,.T.) ;
#4149 = ORIENTED_EDGE('',*,*,#2977,.T.) ;
#4150 = ORIENTED_EDGE('',*,*,#3073,.T.) ;
#4151 = ORIENTED_EDGE('',*,*,#3074,.T.) ;
#4152 = ORIENTED_EDGE('',*,*,#3075,.F.) ;
#4153 = ORIENTED_EDGE('',*,*,#3071,.T.) ;
#4154 = ORIENTED_EDGE('',*,*,#3050,.F.) ;
#4155 = ORIENTED_EDGE('',*,*,#2971,.F.) ;
#4156 = ORIENTED_EDGE('',*,*,#2978,.F.) ;
#4157 = ORIENTED_EDGE('',*,*,#3076,.T.) ;
#4158 = ORIENTED_EDGE('',*,*,#3077,.F.) ;
#4159 = ORIENTED_EDGE('',*,*,#3076,.F.) ;
#4160 = ORIENTED_EDGE('',*,*,#3078,.F.) ;
#4161 = ORIENTED_EDGE('',*,*,#3079,.T.) ;
#4162 = ORIENTED_EDGE('',*,*,#2991,.F.) ;
#4163 = ORIENTED_EDGE('',*,*,#3079,.F.) ;
#4164 = ORIENTED_EDGE('',*,*,#3057,.F.) ;
#4165 = ORIENTED_EDGE('',*,*,#3080,.F.) ;
#4166 = ORIENTED_EDGE('',*,*,#3081,.F.) ;
#4167 = ORIENTED_EDGE('',*,*,#3082,.F.) ;
#4168 = ORIENTED_EDGE('',*,*,#3083,.F.) ;
#4169 = ORIENTED_EDGE('',*,*,#3084,.F.) ;
#4170 = ORIENTED_EDGE('',*,*,#3085,.F.) ;
#4171 = ORIENTED_EDGE('',*,*,#3078,.T.) ;
#4172 = ORIENTED_EDGE('',*,*,#3086,.F.) ;
#4173 = ORIENTED_EDGE('',*,*,#3087,.T.) ;
#4174 = ORIENTED_EDGE('',*,*,#3081,.T.) ;
#4175 = ORIENTED_EDGE('',*,*,#3088,.F.) ;
#4176 = ORIENTED_EDGE('',*,*,#3089,.F.) ;
#4177 = ORIENTED_EDGE('',*,*,#3090,.T.) ;
#4178 = ORIENTED_EDGE('',*,*,#3082,.T.) ;
#4179 = ORIENTED_EDGE('',*,*,#3087,.F.) ;
#4180 = ORIENTED_EDGE('',*,*,#3091,.F.) ;
#4181 = ORIENTED_EDGE('',*,*,#3092,.T.) ;
#4182 = ORIENTED_EDGE('',*,*,#3083,.T.) ;
#4183 = ORIENTED_EDGE('',*,*,#3090,.F.) ;
#4184 = ORIENTED_EDGE('',*,*,#3093,.F.) ;
#4185 = ORIENTED_EDGE('',*,*,#3084,.T.) ;
#4186 = ORIENTED_EDGE('',*,*,#3092,.F.) ;
#4187 = ORIENTED_EDGE('',*,*,#3094,.F.) ;
#4188 = ORIENTED_EDGE('',*,*,#3074,.F.) ;
#4189 = ORIENTED_EDGE('',*,*,#3095,.F.) ;
#4190 = ORIENTED_EDGE('',*,*,#3094,.T.) ;
#4191 = ORIENTED_EDGE('',*,*,#3091,.T.) ;
#4192 = ORIENTED_EDGE('',*,*,#3089,.T.) ;
#4193 = ORIENTED_EDGE('',*,*,#3086,.T.) ;
#4194 = ORIENTED_EDGE('',*,*,#3096,.F.) ;
#4195 = ORIENTED_EDGE('',*,*,#3077,.T.) ;
#4196 = ORIENTED_EDGE('',*,*,#3096,.T.) ;
#4197 = ORIENTED_EDGE('',*,*,#3088,.T.) ;
#4198 = ORIENTED_EDGE('',*,*,#3080,.T.) ;
#4199 = ORIENTED_EDGE('',*,*,#3056,.T.) ;
#4200 = ORIENTED_EDGE('',*,*,#3060,.F.) ;
#4201 = ORIENTED_EDGE('',*,*,#3062,.T.) ;
#4202 = ORIENTED_EDGE('',*,*,#3064,.F.) ;
#4203 = ORIENTED_EDGE('',*,*,#3066,.F.) ;
#4204 = ORIENTED_EDGE('',*,*,#3068,.F.) ;
#4205 = ORIENTED_EDGE('',*,*,#3070,.T.) ;
#4206 = ORIENTED_EDGE('',*,*,#3072,.F.) ;
#4207 = ORIENTED_EDGE('',*,*,#3075,.T.) ;
#4208 = ORIENTED_EDGE('',*,*,#3035,.F.) ;
#4209 = ORIENTED_EDGE('',*,*,#3097,.F.) ;
#4210 = ORIENTED_EDGE('',*,*,#3098,.F.) ;
#4211 = ORIENTED_EDGE('',*,*,#3032,.F.) ;
#4212 = ORIENTED_EDGE('',*,*,#3008,.F.) ;
#4213 = ORIENTED_EDGE('',*,*,#3099,.F.) ;
#4214 = ORIENTED_EDGE('',*,*,#3100,.F.) ;
#4215 = ORIENTED_EDGE('',*,*,#3005,.F.) ;
#4216 = ORIENTED_EDGE('',*,*,#2975,.T.) ;
#4217 = ORIENTED_EDGE('',*,*,#3037,.T.) ;
#4218 = ORIENTED_EDGE('',*,*,#2989,.F.) ;
#4219 = ORIENTED_EDGE('',*,*,#3101,.F.) ;
#4220 = ORIENTED_EDGE('',*,*,#3095,.T.) ;
#4221 = ORIENTED_EDGE('',*,*,#3073,.F.) ;
#4222 = ORIENTED_EDGE('',*,*,#2976,.T.) ;
#4223 = ORIENTED_EDGE('',*,*,#3101,.T.) ;
#4224 = ORIENTED_EDGE('',*,*,#2988,.F.) ;
#4225 = ORIENTED_EDGE('',*,*,#3058,.F.) ;
#4226 = ORIENTED_EDGE('',*,*,#3085,.T.) ;
#4227 = ORIENTED_EDGE('',*,*,#3093,.T.) ;
#4228 = ORIENTED_EDGE('',*,*,#3030,.F.) ;
#4229 = ORIENTED_EDGE('',*,*,#3102,.F.) ;
#4230 = ORIENTED_EDGE('',*,*,#3097,.T.) ;
#4231 = ORIENTED_EDGE('',*,*,#3034,.T.) ;
#4232 = ORIENTED_EDGE('',*,*,#3029,.F.) ;
#4233 = ORIENTED_EDGE('',*,*,#3033,.F.) ;
#4234 = ORIENTED_EDGE('',*,*,#3098,.T.) ;
#4235 = ORIENTED_EDGE('',*,*,#3102,.T.) ;
#4236 = ORIENTED_EDGE('',*,*,#3003,.F.) ;
#4237 = ORIENTED_EDGE('',*,*,#3103,.F.) ;
#4238 = ORIENTED_EDGE('',*,*,#3099,.T.) ;
#4239 = ORIENTED_EDGE('',*,*,#3007,.T.) ;
#4240 = ORIENTED_EDGE('',*,*,#3001,.F.) ;
#4241 = ORIENTED_EDGE('',*,*,#3006,.F.) ;
#4242 = ORIENTED_EDGE('',*,*,#3100,.T.) ;
#4243 = ORIENTED_EDGE('',*,*,#3103,.T.) ;
#4244 = ORIENTED_EDGE('',*,*,#3104,.T.) ;
#4245 = ORIENTED_EDGE('',*,*,#3105,.T.) ;
#4246 = ORIENTED_EDGE('',*,*,#3106,.T.) ;
#4247 = ORIENTED_EDGE('',*,*,#3107,.F.) ;
#4248 = ORIENTED_EDGE('',*,*,#3108,.T.) ;
#4249 = ORIENTED_EDGE('',*,*,#3109,.T.) ;
#4250 = ORIENTED_EDGE('',*,*,#3110,.T.) ;
#4251 = ORIENTED_EDGE('',*,*,#3105,.F.) ;
#4252 = ORIENTED_EDGE('',*,*,#3111,.T.) ;
#4253 = ORIENTED_EDGE('',*,*,#3112,.T.) ;
#4254 = ORIENTED_EDGE('',*,*,#3113,.T.) ;
#4255 = ORIENTED_EDGE('',*,*,#3109,.F.) ;
#4256 = ORIENTED_EDGE('',*,*,#3114,.T.) ;
#4257 = ORIENTED_EDGE('',*,*,#3115,.T.) ;
#4258 = ORIENTED_EDGE('',*,*,#3116,.T.) ;
#4259 = ORIENTED_EDGE('',*,*,#3112,.F.) ;
#4260 = ORIENTED_EDGE('',*,*,#3117,.T.) ;
#4261 = ORIENTED_EDGE('',*,*,#3118,.T.) ;
#4262 = ORIENTED_EDGE('',*,*,#3119,.T.) ;
#4263 = ORIENTED_EDGE('',*,*,#3115,.F.) ;
#4264 = ORIENTED_EDGE('',*,*,#3120,.T.) ;
#4265 = ORIENTED_EDGE('',*,*,#3121,.T.) ;
#4266 = ORIENTED_EDGE('',*,*,#3122,.T.) ;
#4267 = ORIENTED_EDGE('',*,*,#3123,.T.) ;
#4268 = ORIENTED_EDGE('',*,*,#3124,.T.) ;
#4269 = ORIENTED_EDGE('',*,*,#3122,.F.) ;
#4270 = ORIENTED_EDGE('',*,*,#3125,.T.) ;
#4271 = ORIENTED_EDGE('',*,*,#3126,.T.) ;
#4272 = ORIENTED_EDGE('',*,*,#3127,.T.) ;
#4273 = ORIENTED_EDGE('',*,*,#3128,.T.) ;
#4274 = ORIENTED_EDGE('',*,*,#3129,.T.) ;
#4275 = ORIENTED_EDGE('',*,*,#3118,.F.) ;
#4276 = ORIENTED_EDGE('',*,*,#3120,.F.) ;
#4277 = ORIENTED_EDGE('',*,*,#3130,.T.) ;
#4278 = ORIENTED_EDGE('',*,*,#3131,.T.) ;
#4279 = ORIENTED_EDGE('',*,*,#3132,.T.) ;
#4280 = ORIENTED_EDGE('',*,*,#3133,.T.) ;
#4281 = ORIENTED_EDGE('',*,*,#3134,.T.) ;
#4282 = ORIENTED_EDGE('',*,*,#3135,.T.) ;
#4283 = ORIENTED_EDGE('',*,*,#3128,.F.) ;
#4284 = ORIENTED_EDGE('',*,*,#3136,.T.) ;
#4285 = ORIENTED_EDGE('',*,*,#3137,.T.) ;
#4286 = ORIENTED_EDGE('',*,*,#3138,.T.) ;
#4287 = ORIENTED_EDGE('',*,*,#3139,.T.) ;
#4288 = ORIENTED_EDGE('',*,*,#3140,.T.) ;
#4289 = ORIENTED_EDGE('',*,*,#3141,.T.) ;
#4290 = ORIENTED_EDGE('',*,*,#3142,.T.) ;
#4291 = ORIENTED_EDGE('',*,*,#3143,.T.) ;
#4292 = ORIENTED_EDGE('',*,*,#3144,.T.) ;
#4293 = ORIENTED_EDGE('',*,*,#3145,.T.) ;
#4294 = ORIENTED_EDGE('',*,*,#3146,.T.) ;
#4295 = ORIENTED_EDGE('',*,*,#3138,.F.) ;
#4296 = ORIENTED_EDGE('',*,*,#3141,.F.) ;
#4297 = ORIENTED_EDGE('',*,*,#3147,.T.) ;
#4298 = ORIENTED_EDGE('',*,*,#3148,.T.) ;
#4299 = ORIENTED_EDGE('',*,*,#3149,.T.) ;
#4300 = ORIENTED_EDGE('',*,*,#3150,.T.) ;
#4301 = ORIENTED_EDGE('',*,*,#3151,.T.) ;
#4302 = ORIENTED_EDGE('',*,*,#3152,.T.) ;
#4303 = ORIENTED_EDGE('',*,*,#3145,.F.) ;
#4304 = ORIENTED_EDGE('',*,*,#3153,.T.) ;
#4305 = ORIENTED_EDGE('',*,*,#3154,.T.) ;
#4306 = ORIENTED_EDGE('',*,*,#3155,.T.) ;
#4307 = ORIENTED_EDGE('',*,*,#3156,.T.) ;
#4308 = ORIENTED_EDGE('',*,*,#3157,.T.) ;
#4309 = ORIENTED_EDGE('',*,*,#3153,.F.) ;
#4310 = ORIENTED_EDGE('',*,*,#3158,.T.) ;
#4311 = ORIENTED_EDGE('',*,*,#3151,.F.) ;
#4312 = ORIENTED_EDGE('',*,*,#3148,.F.) ;
#4313 = ORIENTED_EDGE('',*,*,#3159,.T.) ;
#4314 = ORIENTED_EDGE('',*,*,#3155,.F.) ;
#4315 = ORIENTED_EDGE('',*,*,#3160,.T.) ;
#4316 = ORIENTED_EDGE('',*,*,#3161,.T.) ;
#4317 = ORIENTED_EDGE('',*,*,#3143,.F.) ;
#4318 = ORIENTED_EDGE('',*,*,#3162,.T.) ;
#4319 = ORIENTED_EDGE('',*,*,#3163,.T.) ;
#4320 = ORIENTED_EDGE('',*,*,#3164,.T.) ;
#4321 = ORIENTED_EDGE('',*,*,#3165,.T.) ;
#4322 = ORIENTED_EDGE('',*,*,#3136,.F.) ;
#4323 = ORIENTED_EDGE('',*,*,#3166,.T.) ;
#4324 = ORIENTED_EDGE('',*,*,#3167,.T.) ;
#4325 = ORIENTED_EDGE('',*,*,#3163,.F.) ;
#4326 = ORIENTED_EDGE('',*,*,#3168,.T.) ;
#4327 = ORIENTED_EDGE('',*,*,#3169,.T.) ;
#4328 = ORIENTED_EDGE('',*,*,#3170,.T.) ;
#4329 = ORIENTED_EDGE('',*,*,#3164,.F.) ;
#4330 = ORIENTED_EDGE('',*,*,#3171,.T.) ;
#4331 = ORIENTED_EDGE('',*,*,#3134,.F.) ;
#4332 = ORIENTED_EDGE('',*,*,#3131,.F.) ;
#4333 = ORIENTED_EDGE('',*,*,#3172,.T.) ;
#4334 = ORIENTED_EDGE('',*,*,#3173,.T.) ;
#4335 = ORIENTED_EDGE('',*,*,#3174,.T.) ;
#4336 = ORIENTED_EDGE('',*,*,#3175,.T.) ;
#4337 = ORIENTED_EDGE('',*,*,#3173,.F.) ;
#4338 = ORIENTED_EDGE('',*,*,#3176,.T.) ;
#4339 = ORIENTED_EDGE('',*,*,#3169,.F.) ;
#4340 = ORIENTED_EDGE('',*,*,#3177,.T.) ;
#4341 = ORIENTED_EDGE('',*,*,#3126,.F.) ;
#4342 = ORIENTED_EDGE('',*,*,#3178,.T.) ;
#4343 = ORIENTED_EDGE('',*,*,#3179,.T.) ;
#4344 = ORIENTED_EDGE('',*,*,#3180,.T.) ;
#4345 = ORIENTED_EDGE('',*,*,#3179,.F.) ;
#4346 = ORIENTED_EDGE('',*,*,#3181,.T.) ;
#4347 = ORIENTED_EDGE('',*,*,#3182,.T.) ;
#4348 = ORIENTED_EDGE('',*,*,#3183,.T.) ;
#4349 = ORIENTED_EDGE('',*,*,#3184,.T.) ;
#4350 = ORIENTED_EDGE('',*,*,#3185,.T.) ;
#4351 = ORIENTED_EDGE('',*,*,#3182,.F.) ;
#4352 = ORIENTED_EDGE('',*,*,#3186,.T.) ;
#4353 = ORIENTED_EDGE('',*,*,#3184,.F.) ;
#4354 = ORIENTED_EDGE('',*,*,#3187,.T.) ;
#4355 = ORIENTED_EDGE('',*,*,#3188,.T.) ;
#4356 = ORIENTED_EDGE('',*,*,#3189,.T.) ;
#4357 = ORIENTED_EDGE('',*,*,#3188,.F.) ;
#4358 = ORIENTED_EDGE('',*,*,#3190,.T.) ;
#4359 = ORIENTED_EDGE('',*,*,#3107,.T.) ;
#4360 = ORIENTED_EDGE('',*,*,#3189,.F.) ;
#4361 = ORIENTED_EDGE('',*,*,#3191,.F.) ;
#4362 = ORIENTED_EDGE('',*,*,#3192,.F.) ;
#4363 = ORIENTED_EDGE('',*,*,#3193,.T.) ;
#4364 = ORIENTED_EDGE('',*,*,#3106,.F.) ;
#4365 = ORIENTED_EDGE('',*,*,#3194,.F.) ;
#4366 = ORIENTED_EDGE('',*,*,#3195,.F.) ;
#4367 = ORIENTED_EDGE('',*,*,#3191,.T.) ;
#4368 = ORIENTED_EDGE('',*,*,#3110,.F.) ;
#4369 = ORIENTED_EDGE('',*,*,#3196,.F.) ;
#4370 = ORIENTED_EDGE('',*,*,#3197,.F.) ;
#4371 = ORIENTED_EDGE('',*,*,#3194,.T.) ;
#4372 = ORIENTED_EDGE('',*,*,#3113,.F.) ;
#4373 = ORIENTED_EDGE('',*,*,#3198,.F.) ;
#4374 = ORIENTED_EDGE('',*,*,#3199,.F.) ;
#4375 = ORIENTED_EDGE('',*,*,#3196,.T.) ;
#4376 = ORIENTED_EDGE('',*,*,#3116,.F.) ;
#4377 = ORIENTED_EDGE('',*,*,#3200,.F.) ;
#4378 = ORIENTED_EDGE('',*,*,#3201,.F.) ;
#4379 = ORIENTED_EDGE('',*,*,#3198,.T.) ;
#4380 = ORIENTED_EDGE('',*,*,#3119,.F.) ;
#4381 = ORIENTED_EDGE('',*,*,#3202,.F.) ;
#4382 = ORIENTED_EDGE('',*,*,#3203,.F.) ;
#4383 = ORIENTED_EDGE('',*,*,#3200,.T.) ;
#4384 = ORIENTED_EDGE('',*,*,#3129,.F.) ;
#4385 = ORIENTED_EDGE('',*,*,#3204,.F.) ;
#4386 = ORIENTED_EDGE('',*,*,#3205,.F.) ;
#4387 = ORIENTED_EDGE('',*,*,#3202,.T.) ;
#4388 = ORIENTED_EDGE('',*,*,#3135,.F.) ;
#4389 = ORIENTED_EDGE('',*,*,#3206,.F.) ;
#4390 = ORIENTED_EDGE('',*,*,#3207,.F.) ;
#4391 = ORIENTED_EDGE('',*,*,#3204,.T.) ;
#4392 = ORIENTED_EDGE('',*,*,#3171,.F.) ;
#4393 = ORIENTED_EDGE('',*,*,#3208,.F.) ;
#4394 = ORIENTED_EDGE('',*,*,#3209,.F.) ;
#4395 = ORIENTED_EDGE('',*,*,#3206,.T.) ;
#4396 = ORIENTED_EDGE('',*,*,#3166,.F.) ;
#4397 = ORIENTED_EDGE('',*,*,#3210,.F.) ;
#4398 = ORIENTED_EDGE('',*,*,#3211,.F.) ;
#4399 = ORIENTED_EDGE('',*,*,#3208,.T.) ;
#4400 = ORIENTED_EDGE('',*,*,#3139,.F.) ;
#4401 = ORIENTED_EDGE('',*,*,#3212,.F.) ;
#4402 = ORIENTED_EDGE('',*,*,#3213,.F.) ;
#4403 = ORIENTED_EDGE('',*,*,#3210,.T.) ;
#4404 = ORIENTED_EDGE('',*,*,#3146,.F.) ;
#4405 = ORIENTED_EDGE('',*,*,#3214,.F.) ;
#4406 = ORIENTED_EDGE('',*,*,#3215,.F.) ;
#4407 = ORIENTED_EDGE('',*,*,#3212,.T.) ;
#4408 = ORIENTED_EDGE('',*,*,#3152,.F.) ;
#4409 = ORIENTED_EDGE('',*,*,#3216,.F.) ;
#4410 = ORIENTED_EDGE('',*,*,#3217,.F.) ;
#4411 = ORIENTED_EDGE('',*,*,#3214,.T.) ;
#4412 = ORIENTED_EDGE('',*,*,#3158,.F.) ;
#4413 = ORIENTED_EDGE('',*,*,#3218,.F.) ;
#4414 = ORIENTED_EDGE('',*,*,#3219,.F.) ;
#4415 = ORIENTED_EDGE('',*,*,#3216,.T.) ;
#4416 = ORIENTED_EDGE('',*,*,#3156,.F.) ;
#4417 = ORIENTED_EDGE('',*,*,#3220,.F.) ;
#4418 = ORIENTED_EDGE('',*,*,#3221,.F.) ;
#4419 = ORIENTED_EDGE('',*,*,#3218,.T.) ;
#4420 = ORIENTED_EDGE('',*,*,#3154,.F.) ;
#4421 = ORIENTED_EDGE('',*,*,#3157,.F.) ;
#4422 = ORIENTED_EDGE('',*,*,#3150,.F.) ;
#4423 = ORIENTED_EDGE('',*,*,#3144,.F.) ;
#4424 = ORIENTED_EDGE('',*,*,#3137,.F.) ;
#4425 = ORIENTED_EDGE('',*,*,#3165,.F.) ;
#4426 = ORIENTED_EDGE('',*,*,#3170,.F.) ;
#4427 = ORIENTED_EDGE('',*,*,#3133,.F.) ;
#4428 = ORIENTED_EDGE('',*,*,#3127,.F.) ;
#4429 = ORIENTED_EDGE('',*,*,#3117,.F.) ;
#4430 = ORIENTED_EDGE('',*,*,#3114,.F.) ;
#4431 = ORIENTED_EDGE('',*,*,#3111,.F.) ;
#4432 = ORIENTED_EDGE('',*,*,#3108,.F.) ;
#4433 = ORIENTED_EDGE('',*,*,#3104,.F.) ;
#4434 = ORIENTED_EDGE('',*,*,#3190,.F.) ;
#4435 = ORIENTED_EDGE('',*,*,#3187,.F.) ;
#4436 = ORIENTED_EDGE('',*,*,#3183,.F.) ;
#4437 = ORIENTED_EDGE('',*,*,#3181,.F.) ;
#4438 = ORIENTED_EDGE('',*,*,#3178,.F.) ;
#4439 = ORIENTED_EDGE('',*,*,#3125,.F.) ;
#4440 = ORIENTED_EDGE('',*,*,#3121,.F.) ;
#4441 = ORIENTED_EDGE('',*,*,#3132,.F.) ;
#4442 = ORIENTED_EDGE('',*,*,#3174,.F.) ;
#4443 = ORIENTED_EDGE('',*,*,#3175,.F.) ;
#4444 = ORIENTED_EDGE('',*,*,#3168,.F.) ;
#4445 = ORIENTED_EDGE('',*,*,#3162,.F.) ;
#4446 = ORIENTED_EDGE('',*,*,#3142,.F.) ;
#4447 = ORIENTED_EDGE('',*,*,#3149,.F.) ;
#4448 = ORIENTED_EDGE('',*,*,#3160,.F.) ;
#4449 = ORIENTED_EDGE('',*,*,#3222,.F.) ;
#4450 = ORIENTED_EDGE('',*,*,#3223,.F.) ;
#4451 = ORIENTED_EDGE('',*,*,#3224,.F.) ;
#4452 = ORIENTED_EDGE('',*,*,#3225,.F.) ;
#4453 = ORIENTED_EDGE('',*,*,#3226,.T.) ;
#4454 = ORIENTED_EDGE('',*,*,#3227,.T.) ;
#4455 = ORIENTED_EDGE('',*,*,#3228,.T.) ;
#4456 = ORIENTED_EDGE('',*,*,#3192,.T.) ;
#4457 = ORIENTED_EDGE('',*,*,#3229,.F.) ;
#4458 = ORIENTED_EDGE('',*,*,#3230,.T.) ;
#4459 = ORIENTED_EDGE('',*,*,#3231,.T.) ;
#4460 = ORIENTED_EDGE('',*,*,#3232,.T.) ;
#4461 = ORIENTED_EDGE('',*,*,#3228,.F.) ;
#4462 = ORIENTED_EDGE('',*,*,#3233,.T.) ;
#4463 = ORIENTED_EDGE('',*,*,#3234,.T.) ;
#4464 = ORIENTED_EDGE('',*,*,#3235,.T.) ;
#4465 = ORIENTED_EDGE('',*,*,#3231,.F.) ;
#4466 = ORIENTED_EDGE('',*,*,#3236,.T.) ;
#4467 = ORIENTED_EDGE('',*,*,#3237,.T.) ;
#4468 = ORIENTED_EDGE('',*,*,#3238,.T.) ;
#4469 = ORIENTED_EDGE('',*,*,#3234,.F.) ;
#4470 = ORIENTED_EDGE('',*,*,#3239,.T.) ;
#4471 = ORIENTED_EDGE('',*,*,#3240,.T.) ;
#4472 = ORIENTED_EDGE('',*,*,#3241,.T.) ;
#4473 = ORIENTED_EDGE('',*,*,#3237,.F.) ;
#4474 = ORIENTED_EDGE('',*,*,#3209,.T.) ;
#4475 = ORIENTED_EDGE('',*,*,#3242,.T.) ;
#4476 = ORIENTED_EDGE('',*,*,#3243,.T.) ;
#4477 = ORIENTED_EDGE('',*,*,#3244,.T.) ;
#4478 = ORIENTED_EDGE('',*,*,#3245,.T.) ;
#4479 = ORIENTED_EDGE('',*,*,#3246,.T.) ;
#4480 = ORIENTED_EDGE('',*,*,#3247,.T.) ;
#4481 = ORIENTED_EDGE('',*,*,#3248,.T.) ;
#4482 = ORIENTED_EDGE('',*,*,#3249,.T.) ;
#4483 = ORIENTED_EDGE('',*,*,#3247,.F.) ;
#4484 = ORIENTED_EDGE('',*,*,#3250,.T.) ;
#4485 = ORIENTED_EDGE('',*,*,#3251,.T.) ;
#4486 = ORIENTED_EDGE('',*,*,#3242,.F.) ;
#4487 = ORIENTED_EDGE('',*,*,#3211,.T.) ;
#4488 = ORIENTED_EDGE('',*,*,#3252,.T.) ;
#4489 = ORIENTED_EDGE('',*,*,#3253,.T.) ;
#4490 = ORIENTED_EDGE('',*,*,#3254,.T.) ;
#4491 = ORIENTED_EDGE('',*,*,#3255,.T.) ;
#4492 = ORIENTED_EDGE('',*,*,#3256,.T.) ;
#4493 = ORIENTED_EDGE('',*,*,#3251,.F.) ;
#4494 = ORIENTED_EDGE('',*,*,#3257,.T.) ;
#4495 = ORIENTED_EDGE('',*,*,#3258,.T.) ;
#4496 = ORIENTED_EDGE('',*,*,#3259,.T.) ;
#4497 = ORIENTED_EDGE('',*,*,#3255,.F.) ;
#4498 = ORIENTED_EDGE('',*,*,#3260,.T.) ;
#4499 = ORIENTED_EDGE('',*,*,#3221,.T.) ;
#4500 = ORIENTED_EDGE('',*,*,#3261,.T.) ;
#4501 = ORIENTED_EDGE('',*,*,#3262,.T.) ;
#4502 = ORIENTED_EDGE('',*,*,#3263,.T.) ;
#4503 = ORIENTED_EDGE('',*,*,#3264,.T.) ;
#4504 = ORIENTED_EDGE('',*,*,#3261,.F.) ;
#4505 = ORIENTED_EDGE('',*,*,#3265,.T.) ;
#4506 = ORIENTED_EDGE('',*,*,#3219,.T.) ;
#4507 = ORIENTED_EDGE('',*,*,#3260,.F.) ;
#4508 = ORIENTED_EDGE('',*,*,#3266,.T.) ;
#4509 = ORIENTED_EDGE('',*,*,#3267,.T.) ;
#4510 = ORIENTED_EDGE('',*,*,#3268,.T.) ;
#4511 = ORIENTED_EDGE('',*,*,#3269,.T.) ;
#4512 = ORIENTED_EDGE('',*,*,#3263,.F.) ;
#4513 = ORIENTED_EDGE('',*,*,#3270,.T.) ;
#4514 = ORIENTED_EDGE('',*,*,#3217,.T.) ;
#4515 = ORIENTED_EDGE('',*,*,#3267,.F.) ;
#4516 = ORIENTED_EDGE('',*,*,#3271,.T.) ;
#4517 = ORIENTED_EDGE('',*,*,#3272,.T.) ;
#4518 = ORIENTED_EDGE('',*,*,#3273,.T.) ;
#4519 = ORIENTED_EDGE('',*,*,#3268,.F.) ;
#4520 = ORIENTED_EDGE('',*,*,#3274,.T.) ;
#4521 = ORIENTED_EDGE('',*,*,#3258,.F.) ;
#4522 = ORIENTED_EDGE('',*,*,#3215,.T.) ;
#4523 = ORIENTED_EDGE('',*,*,#3272,.F.) ;
#4524 = ORIENTED_EDGE('',*,*,#3275,.T.) ;
#4525 = ORIENTED_EDGE('',*,*,#3276,.T.) ;
#4526 = ORIENTED_EDGE('',*,*,#3252,.F.) ;
#4527 = ORIENTED_EDGE('',*,*,#3213,.T.) ;
#4528 = ORIENTED_EDGE('',*,*,#3276,.F.) ;
#4529 = ORIENTED_EDGE('',*,*,#3277,.T.) ;
#4530 = ORIENTED_EDGE('',*,*,#3278,.T.) ;
#4531 = ORIENTED_EDGE('',*,*,#3279,.T.) ;
#4532 = ORIENTED_EDGE('',*,*,#3245,.F.) ;
#4533 = ORIENTED_EDGE('',*,*,#3280,.T.) ;
#4534 = ORIENTED_EDGE('',*,*,#3207,.T.) ;
#4535 = ORIENTED_EDGE('',*,*,#3244,.F.) ;
#4536 = ORIENTED_EDGE('',*,*,#3281,.T.) ;
#4537 = ORIENTED_EDGE('',*,*,#3282,.T.) ;
#4538 = ORIENTED_EDGE('',*,*,#3283,.T.) ;
#4539 = ORIENTED_EDGE('',*,*,#3284,.T.) ;
#4540 = ORIENTED_EDGE('',*,*,#3285,.T.) ;
#4541 = ORIENTED_EDGE('',*,*,#3240,.F.) ;
#4542 = ORIENTED_EDGE('',*,*,#3278,.F.) ;
#4543 = ORIENTED_EDGE('',*,*,#3286,.T.) ;
#4544 = ORIENTED_EDGE('',*,*,#3284,.F.) ;
#4545 = ORIENTED_EDGE('',*,*,#3287,.T.) ;
#4546 = ORIENTED_EDGE('',*,*,#3205,.T.) ;
#4547 = ORIENTED_EDGE('',*,*,#3282,.F.) ;
#4548 = ORIENTED_EDGE('',*,*,#3288,.T.) ;
#4549 = ORIENTED_EDGE('',*,*,#3289,.T.) ;
#4550 = ORIENTED_EDGE('',*,*,#3203,.T.) ;
#4551 = ORIENTED_EDGE('',*,*,#3289,.F.) ;
#4552 = ORIENTED_EDGE('',*,*,#3290,.T.) ;
#4553 = ORIENTED_EDGE('',*,*,#3291,.T.) ;
#4554 = ORIENTED_EDGE('',*,*,#3201,.T.) ;
#4555 = ORIENTED_EDGE('',*,*,#3291,.F.) ;
#4556 = ORIENTED_EDGE('',*,*,#3292,.T.) ;
#4557 = ORIENTED_EDGE('',*,*,#3293,.T.) ;
#4558 = ORIENTED_EDGE('',*,*,#3199,.T.) ;
#4559 = ORIENTED_EDGE('',*,*,#3293,.F.) ;
#4560 = ORIENTED_EDGE('',*,*,#3294,.T.) ;
#4561 = ORIENTED_EDGE('',*,*,#3295,.T.) ;
#4562 = ORIENTED_EDGE('',*,*,#3197,.T.) ;
#4563 = ORIENTED_EDGE('',*,*,#3295,.F.) ;
#4564 = ORIENTED_EDGE('',*,*,#3296,.T.) ;
#4565 = ORIENTED_EDGE('',*,*,#3297,.T.) ;
#4566 = ORIENTED_EDGE('',*,*,#3195,.T.) ;
#4567 = ORIENTED_EDGE('',*,*,#3297,.F.) ;
#4568 = ORIENTED_EDGE('',*,*,#3298,.T.) ;
#4569 = ORIENTED_EDGE('',*,*,#3229,.T.) ;
#4570 = ORIENTED_EDGE('',*,*,#3186,.F.) ;
#4571 = ORIENTED_EDGE('',*,*,#3193,.F.) ;
#4572 = ORIENTED_EDGE('',*,*,#3232,.F.) ;
#4573 = ORIENTED_EDGE('',*,*,#3299,.T.) ;
#4574 = ORIENTED_EDGE('',*,*,#3185,.F.) ;
#4575 = ORIENTED_EDGE('',*,*,#3299,.F.) ;
#4576 = ORIENTED_EDGE('',*,*,#3235,.F.) ;
#4577 = ORIENTED_EDGE('',*,*,#3300,.T.) ;
#4578 = ORIENTED_EDGE('',*,*,#3180,.F.) ;
#4579 = ORIENTED_EDGE('',*,*,#3300,.F.) ;
#4580 = ORIENTED_EDGE('',*,*,#3238,.F.) ;
#4581 = ORIENTED_EDGE('',*,*,#3301,.T.) ;
#4582 = ORIENTED_EDGE('',*,*,#3177,.F.) ;
#4583 = ORIENTED_EDGE('',*,*,#3301,.F.) ;
#4584 = ORIENTED_EDGE('',*,*,#3241,.F.) ;
#4585 = ORIENTED_EDGE('',*,*,#3302,.T.) ;
#4586 = ORIENTED_EDGE('',*,*,#3124,.F.) ;
#4587 = ORIENTED_EDGE('',*,*,#3302,.F.) ;
#4588 = ORIENTED_EDGE('',*,*,#3285,.F.) ;
#4589 = ORIENTED_EDGE('',*,*,#3303,.T.) ;
#4590 = ORIENTED_EDGE('',*,*,#3123,.F.) ;
#4591 = ORIENTED_EDGE('',*,*,#3303,.F.) ;
#4592 = ORIENTED_EDGE('',*,*,#3286,.F.) ;
#4593 = ORIENTED_EDGE('',*,*,#3304,.T.) ;
#4594 = ORIENTED_EDGE('',*,*,#3130,.F.) ;
#4595 = ORIENTED_EDGE('',*,*,#3304,.F.) ;
#4596 = ORIENTED_EDGE('',*,*,#3280,.F.) ;
#4597 = ORIENTED_EDGE('',*,*,#3305,.T.) ;
#4598 = ORIENTED_EDGE('',*,*,#3172,.F.) ;
#4599 = ORIENTED_EDGE('',*,*,#3305,.F.) ;
#4600 = ORIENTED_EDGE('',*,*,#3248,.F.) ;
#4601 = ORIENTED_EDGE('',*,*,#3306,.T.) ;
#4602 = ORIENTED_EDGE('',*,*,#3176,.F.) ;
#4603 = ORIENTED_EDGE('',*,*,#3306,.F.) ;
#4604 = ORIENTED_EDGE('',*,*,#3249,.F.) ;
#4605 = ORIENTED_EDGE('',*,*,#3307,.T.) ;
#4606 = ORIENTED_EDGE('',*,*,#3167,.F.) ;
#4607 = ORIENTED_EDGE('',*,*,#3307,.F.) ;
#4608 = ORIENTED_EDGE('',*,*,#3256,.F.) ;
#4609 = ORIENTED_EDGE('',*,*,#3308,.T.) ;
#4610 = ORIENTED_EDGE('',*,*,#3161,.F.) ;
#4611 = ORIENTED_EDGE('',*,*,#3308,.F.) ;
#4612 = ORIENTED_EDGE('',*,*,#3259,.F.) ;
#4613 = ORIENTED_EDGE('',*,*,#3309,.T.) ;
#4614 = ORIENTED_EDGE('',*,*,#3140,.F.) ;
#4615 = ORIENTED_EDGE('',*,*,#3309,.F.) ;
#4616 = ORIENTED_EDGE('',*,*,#3274,.F.) ;
#4617 = ORIENTED_EDGE('',*,*,#3310,.T.) ;
#4618 = ORIENTED_EDGE('',*,*,#3147,.F.) ;
#4619 = ORIENTED_EDGE('',*,*,#3310,.F.) ;
#4620 = ORIENTED_EDGE('',*,*,#3270,.F.) ;
#4621 = ORIENTED_EDGE('',*,*,#3311,.T.) ;
#4622 = ORIENTED_EDGE('',*,*,#3159,.F.) ;
#4623 = ORIENTED_EDGE('',*,*,#3311,.F.) ;
#4624 = ORIENTED_EDGE('',*,*,#3265,.F.) ;
#4625 = ORIENTED_EDGE('',*,*,#3220,.T.) ;
#4626 = ORIENTED_EDGE('',*,*,#3262,.F.) ;
#4627 = ORIENTED_EDGE('',*,*,#3264,.F.) ;
#4628 = ORIENTED_EDGE('',*,*,#3269,.F.) ;
#4629 = ORIENTED_EDGE('',*,*,#3273,.F.) ;
#4630 = ORIENTED_EDGE('',*,*,#3257,.F.) ;
#4631 = ORIENTED_EDGE('',*,*,#3254,.F.) ;
#4632 = ORIENTED_EDGE('',*,*,#3250,.F.) ;
#4633 = ORIENTED_EDGE('',*,*,#3246,.F.) ;
#4634 = ORIENTED_EDGE('',*,*,#3279,.F.) ;
#4635 = ORIENTED_EDGE('',*,*,#3287,.F.) ;
#4636 = ORIENTED_EDGE('',*,*,#3283,.F.) ;
#4637 = ORIENTED_EDGE('',*,*,#3239,.F.) ;
#4638 = ORIENTED_EDGE('',*,*,#3236,.F.) ;
#4639 = ORIENTED_EDGE('',*,*,#3233,.F.) ;
#4640 = ORIENTED_EDGE('',*,*,#3230,.F.) ;
#4641 = ORIENTED_EDGE('',*,*,#3227,.F.) ;
#4642 = ORIENTED_EDGE('',*,*,#3298,.F.) ;
#4643 = ORIENTED_EDGE('',*,*,#3296,.F.) ;
#4644 = ORIENTED_EDGE('',*,*,#3294,.F.) ;
#4645 = ORIENTED_EDGE('',*,*,#3292,.F.) ;
#4646 = ORIENTED_EDGE('',*,*,#3290,.F.) ;
#4647 = ORIENTED_EDGE('',*,*,#3288,.F.) ;
#4648 = ORIENTED_EDGE('',*,*,#3281,.F.) ;
#4649 = ORIENTED_EDGE('',*,*,#3243,.F.) ;
#4650 = ORIENTED_EDGE('',*,*,#3253,.F.) ;
#4651 = ORIENTED_EDGE('',*,*,#3277,.F.) ;
#4652 = ORIENTED_EDGE('',*,*,#3275,.F.) ;
#4653 = ORIENTED_EDGE('',*,*,#3271,.F.) ;
#4654 = ORIENTED_EDGE('',*,*,#3266,.F.) ;
#4655 = ORIENTED_EDGE('',*,*,#3312,.F.) ;
#4656 = ORIENTED_EDGE('',*,*,#3313,.F.) ;
#4657 = ORIENTED_EDGE('',*,*,#3314,.F.) ;
#4658 = ORIENTED_EDGE('',*,*,#3315,.F.) ;
#4659 = ORIENTED_EDGE('',*,*,#3316,.F.) ;
#4660 = ORIENTED_EDGE('',*,*,#3222,.T.) ;
#4661 = ORIENTED_EDGE('',*,*,#3317,.T.) ;
#4662 = ORIENTED_EDGE('',*,*,#3318,.T.) ;
#4663 = ORIENTED_EDGE('',*,*,#3319,.F.) ;
#4664 = ORIENTED_EDGE('',*,*,#3225,.T.) ;
#4665 = ORIENTED_EDGE('',*,*,#3320,.T.) ;
#4666 = ORIENTED_EDGE('',*,*,#3321,.T.) ;
#4667 = ORIENTED_EDGE('',*,*,#3317,.F.) ;
#4668 = ORIENTED_EDGE('',*,*,#3224,.T.) ;
#4669 = ORIENTED_EDGE('',*,*,#3322,.T.) ;
#4670 = ORIENTED_EDGE('',*,*,#3323,.T.) ;
#4671 = ORIENTED_EDGE('',*,*,#3320,.F.) ;
#4672 = ORIENTED_EDGE('',*,*,#3324,.T.) ;
#4673 = ORIENTED_EDGE('',*,*,#3322,.F.) ;
#4674 = ORIENTED_EDGE('',*,*,#3223,.T.) ;
#4675 = ORIENTED_EDGE('',*,*,#3319,.T.) ;
#4676 = ORIENTED_EDGE('',*,*,#3324,.F.) ;
#4677 = ORIENTED_EDGE('',*,*,#3325,.F.) ;
#4678 = ORIENTED_EDGE('',*,*,#3326,.F.) ;
#4679 = ORIENTED_EDGE('',*,*,#3327,.T.) ;
#4680 = ORIENTED_EDGE('',*,*,#3318,.F.) ;
#4681 = ORIENTED_EDGE('',*,*,#3328,.F.) ;
#4682 = ORIENTED_EDGE('',*,*,#3329,.F.) ;
#4683 = ORIENTED_EDGE('',*,*,#3325,.T.) ;
#4684 = ORIENTED_EDGE('',*,*,#3330,.T.) ;
#4685 = ORIENTED_EDGE('',*,*,#3331,.T.) ;
#4686 = ORIENTED_EDGE('',*,*,#3314,.T.) ;
#4687 = ORIENTED_EDGE('',*,*,#3332,.T.) ;
#4688 = ORIENTED_EDGE('',*,*,#3312,.T.) ;
#4689 = ORIENTED_EDGE('',*,*,#3333,.T.) ;
#4690 = ORIENTED_EDGE('',*,*,#3326,.T.) ;
#4691 = ORIENTED_EDGE('',*,*,#3334,.F.) ;
#4692 = ORIENTED_EDGE('',*,*,#3335,.T.) ;
#4693 = ORIENTED_EDGE('',*,*,#3333,.F.) ;
#4694 = ORIENTED_EDGE('',*,*,#3315,.T.) ;
#4695 = ORIENTED_EDGE('',*,*,#3331,.F.) ;
#4696 = ORIENTED_EDGE('',*,*,#3329,.T.) ;
#4697 = ORIENTED_EDGE('',*,*,#3332,.F.) ;
#4698 = ORIENTED_EDGE('',*,*,#3313,.T.) ;
#4699 = ORIENTED_EDGE('',*,*,#3334,.T.) ;
#4700 = ORIENTED_EDGE('',*,*,#3226,.F.) ;
#4701 = ORIENTED_EDGE('',*,*,#3336,.T.) ;
#4702 = ORIENTED_EDGE('',*,*,#3316,.T.) ;
#4703 = ORIENTED_EDGE('',*,*,#3336,.F.) ;
#4704 = ORIENTED_EDGE('',*,*,#3323,.F.) ;
#4705 = ORIENTED_EDGE('',*,*,#3327,.F.) ;
#4706 = ORIENTED_EDGE('',*,*,#3335,.F.) ;
#4707 = ORIENTED_EDGE('',*,*,#3337,.T.) ;
#4708 = ORIENTED_EDGE('',*,*,#3321,.F.) ;
#4709 = ORIENTED_EDGE('',*,*,#3337,.F.) ;
#4710 = ORIENTED_EDGE('',*,*,#3330,.F.) ;
#4711 = ORIENTED_EDGE('',*,*,#3328,.T.) ;
#4712 = ORIENTED_EDGE('',*,*,#3338,.F.) ;
#4713 = ORIENTED_EDGE('',*,*,#3339,.F.) ;
#4714 = ORIENTED_EDGE('',*,*,#3340,.T.) ;
#4715 = ORIENTED_EDGE('',*,*,#3338,.T.) ;
#4716 = ORIENTED_EDGE('',*,*,#3340,.F.) ;
#4717 = ORIENTED_EDGE('',*,*,#3341,.F.) ;
#4718 = ORIENTED_EDGE('',*,*,#3342,.T.) ;
#4719 = ORIENTED_EDGE('',*,*,#3339,.T.) ;
#4720 = ORIENTED_EDGE('',*,*,#3342,.F.) ;
#4721 = ORIENTED_EDGE('',*,*,#3343,.F.) ;
#4722 = ORIENTED_EDGE('',*,*,#3344,.T.) ;
#4723 = ORIENTED_EDGE('',*,*,#3341,.T.) ;
#4724 = ORIENTED_EDGE('',*,*,#3344,.F.) ;
#4725 = ORIENTED_EDGE('',*,*,#3343,.T.) ;
#4726 = ORIENTED_EDGE('',*,*,#3345,.F.) ;
#4727 = ORIENTED_EDGE('',*,*,#3346,.F.) ;
#4728 = ORIENTED_EDGE('',*,*,#3347,.T.) ;
#4729 = ORIENTED_EDGE('',*,*,#3345,.T.) ;
#4730 = ORIENTED_EDGE('',*,*,#3347,.F.) ;
#4731 = ORIENTED_EDGE('',*,*,#3348,.F.) ;
#4732 = ORIENTED_EDGE('',*,*,#3346,.T.) ;
#4733 = ORIENTED_EDGE('',*,*,#3349,.F.) ;
#4734 = ORIENTED_EDGE('',*,*,#3350,.T.) ;
#4735 = ORIENTED_EDGE('',*,*,#3348,.T.) ;
#4736 = ORIENTED_EDGE('',*,*,#3350,.F.) ;
#4737 = ORIENTED_EDGE('',*,*,#3351,.F.) ;
#4738 = ORIENTED_EDGE('',*,*,#3352,.T.) ;
#4739 = ORIENTED_EDGE('',*,*,#3349,.T.) ;
#4740 = ORIENTED_EDGE('',*,*,#3352,.F.) ;
#4741 = ORIENTED_EDGE('',*,*,#3353,.F.) ;
#4742 = ORIENTED_EDGE('',*,*,#3354,.T.) ;
#4743 = ORIENTED_EDGE('',*,*,#3351,.T.) ;
#4744 = ORIENTED_EDGE('',*,*,#3354,.F.) ;
#4745 = ORIENTED_EDGE('',*,*,#3353,.T.) ;
#4746 = ORIENTED_EDGE('',*,*,#3355,.F.) ;
#4747 = ORIENTED_EDGE('',*,*,#3356,.F.) ;
#4748 = ORIENTED_EDGE('',*,*,#3357,.T.) ;
#4749 = ORIENTED_EDGE('',*,*,#3355,.T.) ;
#4750 = ORIENTED_EDGE('',*,*,#3357,.F.) ;
#4751 = ORIENTED_EDGE('',*,*,#3356,.T.) ;
#4752 = ORIENTED_EDGE('',*,*,#3358,.F.) ;
#4753 = ORIENTED_EDGE('',*,*,#3359,.F.) ;
#4754 = ORIENTED_EDGE('',*,*,#3360,.T.) ;
#4755 = ORIENTED_EDGE('',*,*,#3358,.T.) ;
#4756 = ORIENTED_EDGE('',*,*,#3360,.F.) ;
#4757 = ORIENTED_EDGE('',*,*,#3361,.F.) ;
#4758 = ORIENTED_EDGE('',*,*,#3362,.T.) ;
#4759 = ORIENTED_EDGE('',*,*,#3359,.T.) ;
#4760 = ORIENTED_EDGE('',*,*,#3362,.F.) ;
#4761 = ORIENTED_EDGE('',*,*,#3363,.F.) ;
#4762 = ORIENTED_EDGE('',*,*,#3364,.T.) ;
#4763 = ORIENTED_EDGE('',*,*,#3361,.T.) ;
#4764 = ORIENTED_EDGE('',*,*,#3364,.F.) ;
#4765 = ORIENTED_EDGE('',*,*,#3363,.T.) ;
#4766 = ORIENTED_EDGE('',*,*,#3365,.F.) ;
#4767 = ORIENTED_EDGE('',*,*,#3366,.T.) ;
#4768 = ORIENTED_EDGE('',*,*,#3367,.T.) ;
#4769 = ORIENTED_EDGE('',*,*,#3366,.F.) ;
#4770 = ORIENTED_EDGE('',*,*,#3368,.T.) ;
#4771 = ORIENTED_EDGE('',*,*,#3369,.T.) ;
#4772 = ORIENTED_EDGE('',*,*,#3370,.F.) ;
#4773 = ORIENTED_EDGE('',*,*,#3371,.F.) ;
#4774 = ORIENTED_EDGE('',*,*,#3372,.T.) ;
#4775 = ORIENTED_EDGE('',*,*,#3371,.T.) ;
#4776 = ORIENTED_EDGE('',*,*,#3373,.F.) ;
#4777 = ORIENTED_EDGE('',*,*,#3374,.F.) ;
#4778 = ORIENTED_EDGE('',*,*,#3375,.T.) ;
#4779 = ORIENTED_EDGE('',*,*,#3374,.T.) ;
#4780 = ORIENTED_EDGE('',*,*,#3376,.F.) ;
#4781 = ORIENTED_EDGE('',*,*,#3377,.F.) ;
#4782 = ORIENTED_EDGE('',*,*,#3378,.T.) ;
#4783 = ORIENTED_EDGE('',*,*,#3377,.T.) ;
#4784 = ORIENTED_EDGE('',*,*,#3379,.F.) ;
#4785 = ORIENTED_EDGE('',*,*,#3380,.F.) ;
#4786 = ORIENTED_EDGE('',*,*,#3381,.T.) ;
#4787 = ORIENTED_EDGE('',*,*,#3380,.T.) ;
#4788 = ORIENTED_EDGE('',*,*,#3382,.F.) ;
#4789 = ORIENTED_EDGE('',*,*,#3383,.F.) ;
#4790 = ORIENTED_EDGE('',*,*,#3384,.T.) ;
#4791 = ORIENTED_EDGE('',*,*,#3383,.T.) ;
#4792 = ORIENTED_EDGE('',*,*,#3385,.F.) ;
#4793 = ORIENTED_EDGE('',*,*,#3386,.F.) ;
#4794 = ORIENTED_EDGE('',*,*,#3387,.T.) ;
#4795 = ORIENTED_EDGE('',*,*,#3386,.T.) ;
#4796 = ORIENTED_EDGE('',*,*,#3388,.F.) ;
#4797 = ORIENTED_EDGE('',*,*,#3389,.F.) ;
#4798 = ORIENTED_EDGE('',*,*,#3390,.T.) ;
#4799 = ORIENTED_EDGE('',*,*,#3389,.T.) ;
#4800 = ORIENTED_EDGE('',*,*,#3391,.F.) ;
#4801 = ORIENTED_EDGE('',*,*,#3392,.F.) ;
#4802 = ORIENTED_EDGE('',*,*,#3393,.T.) ;
#4803 = ORIENTED_EDGE('',*,*,#3392,.T.) ;
#4804 = ORIENTED_EDGE('',*,*,#3394,.F.) ;
#4805 = ORIENTED_EDGE('',*,*,#3369,.F.) ;
#4806 = ORIENTED_EDGE('',*,*,#3394,.T.) ;
#4807 = ORIENTED_EDGE('',*,*,#3391,.T.) ;
#4808 = ORIENTED_EDGE('',*,*,#3388,.T.) ;
#4809 = ORIENTED_EDGE('',*,*,#3385,.T.) ;
#4810 = ORIENTED_EDGE('',*,*,#3382,.T.) ;
#4811 = ORIENTED_EDGE('',*,*,#3379,.T.) ;
#4812 = ORIENTED_EDGE('',*,*,#3376,.T.) ;
#4813 = ORIENTED_EDGE('',*,*,#3373,.T.) ;
#4814 = ORIENTED_EDGE('',*,*,#3370,.T.) ;
#4815 = ORIENTED_EDGE('',*,*,#3365,.T.) ;
#4816 = ORIENTED_EDGE('',*,*,#3393,.F.) ;
#4817 = ORIENTED_EDGE('',*,*,#3368,.F.) ;
#4818 = ORIENTED_EDGE('',*,*,#3372,.F.) ;
#4819 = ORIENTED_EDGE('',*,*,#3375,.F.) ;
#4820 = ORIENTED_EDGE('',*,*,#3378,.F.) ;
#4821 = ORIENTED_EDGE('',*,*,#3381,.F.) ;
#4822 = ORIENTED_EDGE('',*,*,#3384,.F.) ;
#4823 = ORIENTED_EDGE('',*,*,#3387,.F.) ;
#4824 = ORIENTED_EDGE('',*,*,#3390,.F.) ;
#4825 = ORIENTED_EDGE('',*,*,#3367,.F.) ;
#4826 = ORIENTED_EDGE('',*,*,#3395,.F.) ;
#4827 = ORIENTED_EDGE('',*,*,#3396,.T.) ;
#4828 = ORIENTED_EDGE('',*,*,#3397,.T.) ;
#4829 = ORIENTED_EDGE('',*,*,#3398,.F.) ;
#4830 = ORIENTED_EDGE('',*,*,#3399,.F.) ;
#4831 = ORIENTED_EDGE('',*,*,#3398,.T.) ;
#4832 = ORIENTED_EDGE('',*,*,#3400,.T.) ;
#4833 = ORIENTED_EDGE('',*,*,#3401,.F.) ;
#4834 = ORIENTED_EDGE('',*,*,#3402,.F.) ;
#4835 = ORIENTED_EDGE('',*,*,#3401,.T.) ;
#4836 = ORIENTED_EDGE('',*,*,#3403,.T.) ;
#4837 = ORIENTED_EDGE('',*,*,#3404,.F.) ;
#4838 = ORIENTED_EDGE('',*,*,#3405,.F.) ;
#4839 = ORIENTED_EDGE('',*,*,#3404,.T.) ;
#4840 = ORIENTED_EDGE('',*,*,#3406,.T.) ;
#4841 = ORIENTED_EDGE('',*,*,#3407,.T.) ;
#4842 = ORIENTED_EDGE('',*,*,#3408,.F.) ;
#4843 = ORIENTED_EDGE('',*,*,#3409,.T.) ;
#4844 = ORIENTED_EDGE('',*,*,#3410,.T.) ;
#4845 = ORIENTED_EDGE('',*,*,#3396,.F.) ;
#4846 = ORIENTED_EDGE('',*,*,#3411,.F.) ;
#4847 = ORIENTED_EDGE('',*,*,#3407,.F.) ;
#4848 = ORIENTED_EDGE('',*,*,#3412,.T.) ;
#4849 = ORIENTED_EDGE('',*,*,#3409,.F.) ;
#4850 = ORIENTED_EDGE('',*,*,#3412,.F.) ;
#4851 = ORIENTED_EDGE('',*,*,#3406,.F.) ;
#4852 = ORIENTED_EDGE('',*,*,#3403,.F.) ;
#4853 = ORIENTED_EDGE('',*,*,#3400,.F.) ;
#4854 = ORIENTED_EDGE('',*,*,#3397,.F.) ;
#4855 = ORIENTED_EDGE('',*,*,#3410,.F.) ;
#4856 = ORIENTED_EDGE('',*,*,#3413,.F.) ;
#4857 = ORIENTED_EDGE('',*,*,#3405,.T.) ;
#4858 = ORIENTED_EDGE('',*,*,#3411,.T.) ;
#4859 = ORIENTED_EDGE('',*,*,#3408,.T.) ;
#4860 = ORIENTED_EDGE('',*,*,#3395,.T.) ;
#4861 = ORIENTED_EDGE('',*,*,#3399,.T.) ;
#4862 = ORIENTED_EDGE('',*,*,#3402,.T.) ;
#4863 = ORIENTED_EDGE('',*,*,#3414,.F.) ;
#4864 = ORIENTED_EDGE('',*,*,#3415,.T.) ;
#4865 = ORIENTED_EDGE('',*,*,#3413,.T.) ;
#4866 = ORIENTED_EDGE('',*,*,#3415,.F.) ;
#4867 = ORIENTED_EDGE('',*,*,#3416,.F.) ;
#4868 = ORIENTED_EDGE('',*,*,#3417,.T.) ;
#4869 = ORIENTED_EDGE('',*,*,#3414,.T.) ;
#4870 = ORIENTED_EDGE('',*,*,#3417,.F.) ;
#4871 = ORIENTED_EDGE('',*,*,#3418,.F.) ;
#4872 = ORIENTED_EDGE('',*,*,#3419,.T.) ;
#4873 = ORIENTED_EDGE('',*,*,#3416,.T.) ;
#4874 = ORIENTED_EDGE('',*,*,#3419,.F.) ;
#4875 = ORIENTED_EDGE('',*,*,#3420,.F.) ;
#4876 = ORIENTED_EDGE('',*,*,#3421,.T.) ;
#4877 = ORIENTED_EDGE('',*,*,#3418,.T.) ;
#4878 = ORIENTED_EDGE('',*,*,#3421,.F.) ;
#4879 = ORIENTED_EDGE('',*,*,#3422,.F.) ;
#4880 = ORIENTED_EDGE('',*,*,#3423,.T.) ;
#4881 = ORIENTED_EDGE('',*,*,#3420,.T.) ;
#4882 = ORIENTED_EDGE('',*,*,#3423,.F.) ;
#4883 = ORIENTED_EDGE('',*,*,#3422,.T.) ;
#4884 = ORIENTED_EDGE('',*,*,#3424,.F.) ;
#4885 = ORIENTED_EDGE('',*,*,#3425,.T.) ;
#4886 = ORIENTED_EDGE('',*,*,#3426,.F.) ;
#4887 = ORIENTED_EDGE('',*,*,#3427,.F.) ;
#4888 = ORIENTED_EDGE('',*,*,#3428,.F.) ;
#4889 = ORIENTED_EDGE('',*,*,#3429,.F.) ;
#4890 = ORIENTED_EDGE('',*,*,#3425,.F.) ;
#4891 = ORIENTED_EDGE('',*,*,#3430,.T.) ;
#4892 = ORIENTED_EDGE('',*,*,#3424,.T.) ;
#4893 = ORIENTED_EDGE('',*,*,#3430,.F.) ;
#4894 = ORIENTED_EDGE('',*,*,#3431,.F.) ;
#4895 = ORIENTED_EDGE('',*,*,#3432,.T.) ;
#4896 = ORIENTED_EDGE('',*,*,#3433,.F.) ;
#4897 = ORIENTED_EDGE('',*,*,#3428,.T.) ;
#4898 = ORIENTED_EDGE('',*,*,#3427,.T.) ;
#4899 = ORIENTED_EDGE('',*,*,#3434,.F.) ;
#4900 = ORIENTED_EDGE('',*,*,#3432,.F.) ;
#4901 = ORIENTED_EDGE('',*,*,#3426,.T.) ;
#4902 = ORIENTED_EDGE('',*,*,#3429,.T.) ;
#4903 = ORIENTED_EDGE('',*,*,#3433,.T.) ;
#4904 = ORIENTED_EDGE('',*,*,#3435,.T.) ;
#4905 = ORIENTED_EDGE('',*,*,#3436,.F.) ;
#4906 = ORIENTED_EDGE('',*,*,#3437,.T.) ;
#4907 = ORIENTED_EDGE('',*,*,#3438,.F.) ;
#4908 = ORIENTED_EDGE('',*,*,#3435,.F.) ;
#4909 = ORIENTED_EDGE('',*,*,#3434,.T.) ;
#4910 = ORIENTED_EDGE('',*,*,#3439,.F.) ;
#4911 = ORIENTED_EDGE('',*,*,#3440,.T.) ;
#4912 = ORIENTED_EDGE('',*,*,#3441,.F.) ;
#4913 = ORIENTED_EDGE('',*,*,#3437,.F.) ;
#4914 = ORIENTED_EDGE('',*,*,#3442,.F.) ;
#4915 = ORIENTED_EDGE('',*,*,#3440,.F.) ;
#4916 = ORIENTED_EDGE('',*,*,#3443,.T.) ;
#4917 = ORIENTED_EDGE('',*,*,#3439,.T.) ;
#4918 = ORIENTED_EDGE('',*,*,#3443,.F.) ;
#4919 = ORIENTED_EDGE('',*,*,#3444,.F.) ;
#4920 = ORIENTED_EDGE('',*,*,#3445,.T.) ;
#4921 = ORIENTED_EDGE('',*,*,#3431,.T.) ;
#4922 = ORIENTED_EDGE('',*,*,#3445,.F.) ;
#4923 = ORIENTED_EDGE('',*,*,#3442,.T.) ;
#4924 = ORIENTED_EDGE('',*,*,#3436,.T.) ;
#4925 = ORIENTED_EDGE('',*,*,#3446,.T.) ;
#4926 = ORIENTED_EDGE('',*,*,#3444,.T.) ;
#4927 = ORIENTED_EDGE('',*,*,#3446,.F.) ;
#4928 = ORIENTED_EDGE('',*,*,#3438,.T.) ;
#4929 = ORIENTED_EDGE('',*,*,#3441,.T.) ;
#4930 = ORIENTED_EDGE('',*,*,#3447,.T.) ;
#4931 = ORIENTED_EDGE('',*,*,#3448,.T.) ;
#4932 = ORIENTED_EDGE('',*,*,#3449,.F.) ;
#4933 = ORIENTED_EDGE('',*,*,#3448,.F.) ;
#4934 = ORIENTED_EDGE('',*,*,#3450,.F.) ;
#4935 = ORIENTED_EDGE('',*,*,#3449,.T.) ;
#4936 = ORIENTED_EDGE('',*,*,#3451,.F.) ;
#4937 = ORIENTED_EDGE('',*,*,#3452,.T.) ;
#4938 = ORIENTED_EDGE('',*,*,#3450,.T.) ;
#4939 = ORIENTED_EDGE('',*,*,#3452,.F.) ;
#4940 = ORIENTED_EDGE('',*,*,#3451,.T.) ;
#4941 = ORIENTED_EDGE('',*,*,#3447,.F.) ;
#4942 = ORIENTED_EDGE('',*,*,#3453,.T.) ;
#4943 = ORIENTED_EDGE('',*,*,#3454,.T.) ;
#4944 = ORIENTED_EDGE('',*,*,#3455,.F.) ;
#4945 = ORIENTED_EDGE('',*,*,#3454,.F.) ;
#4946 = ORIENTED_EDGE('',*,*,#3456,.F.) ;
#4947 = ORIENTED_EDGE('',*,*,#3455,.T.) ;
#4948 = ORIENTED_EDGE('',*,*,#3457,.F.) ;
#4949 = ORIENTED_EDGE('',*,*,#3458,.T.) ;
#4950 = ORIENTED_EDGE('',*,*,#3456,.T.) ;
#4951 = ORIENTED_EDGE('',*,*,#3458,.F.) ;
#4952 = ORIENTED_EDGE('',*,*,#3457,.T.) ;
#4953 = ORIENTED_EDGE('',*,*,#3453,.F.) ;
#4954 = ORIENTED_EDGE('',*,*,#3459,.T.) ;
#4955 = ORIENTED_EDGE('',*,*,#3460,.T.) ;
#4956 = ORIENTED_EDGE('',*,*,#3461,.F.) ;
#4957 = ORIENTED_EDGE('',*,*,#3460,.F.) ;
#4958 = ORIENTED_EDGE('',*,*,#3462,.F.) ;
#4959 = ORIENTED_EDGE('',*,*,#3461,.T.) ;
#4960 = ORIENTED_EDGE('',*,*,#3463,.F.) ;
#4961 = ORIENTED_EDGE('',*,*,#3464,.T.) ;
#4962 = ORIENTED_EDGE('',*,*,#3462,.T.) ;
#4963 = ORIENTED_EDGE('',*,*,#3464,.F.) ;
#4964 = ORIENTED_EDGE('',*,*,#3463,.T.) ;
#4965 = ORIENTED_EDGE('',*,*,#3459,.F.) ;
#4966 = ORIENTED_EDGE('',*,*,#3465,.F.) ;
#4967 = ORIENTED_EDGE('',*,*,#3466,.T.) ;
#4968 = ORIENTED_EDGE('',*,*,#3467,.F.) ;
#4969 = ORIENTED_EDGE('',*,*,#3468,.F.) ;
#4970 = ORIENTED_EDGE('',*,*,#3469,.T.) ;
#4971 = ORIENTED_EDGE('',*,*,#3468,.T.) ;
#4972 = ORIENTED_EDGE('',*,*,#3470,.F.) ;
#4973 = ORIENTED_EDGE('',*,*,#3471,.F.) ;
#4974 = ORIENTED_EDGE('',*,*,#3472,.T.) ;
#4975 = ORIENTED_EDGE('',*,*,#3471,.T.) ;
#4976 = ORIENTED_EDGE('',*,*,#3473,.F.) ;
#4977 = ORIENTED_EDGE('',*,*,#3474,.F.) ;
#4978 = ORIENTED_EDGE('',*,*,#3475,.F.) ;
#4979 = ORIENTED_EDGE('',*,*,#3474,.T.) ;
#4980 = ORIENTED_EDGE('',*,*,#3476,.F.) ;
#4981 = ORIENTED_EDGE('',*,*,#3477,.F.) ;
#4982 = ORIENTED_EDGE('',*,*,#3478,.T.) ;
#4983 = ORIENTED_EDGE('',*,*,#3477,.T.) ;
#4984 = ORIENTED_EDGE('',*,*,#3479,.F.) ;
#4985 = ORIENTED_EDGE('',*,*,#3480,.F.) ;
#4986 = ORIENTED_EDGE('',*,*,#3481,.T.) ;
#4987 = ORIENTED_EDGE('',*,*,#3480,.T.) ;
#4988 = ORIENTED_EDGE('',*,*,#3482,.F.) ;
#4989 = ORIENTED_EDGE('',*,*,#3483,.F.) ;
#4990 = ORIENTED_EDGE('',*,*,#3484,.T.) ;
#4991 = ORIENTED_EDGE('',*,*,#3483,.T.) ;
#4992 = ORIENTED_EDGE('',*,*,#3485,.F.) ;
#4993 = ORIENTED_EDGE('',*,*,#3486,.F.) ;
#4994 = ORIENTED_EDGE('',*,*,#3487,.T.) ;
#4995 = ORIENTED_EDGE('',*,*,#3486,.T.) ;
#4996 = ORIENTED_EDGE('',*,*,#3488,.F.) ;
#4997 = ORIENTED_EDGE('',*,*,#3466,.F.) ;
#4998 = ORIENTED_EDGE('',*,*,#3488,.T.) ;
#4999 = ORIENTED_EDGE('',*,*,#3485,.T.) ;
#5000 = ORIENTED_EDGE('',*,*,#3482,.T.) ;
#5001 = ORIENTED_EDGE('',*,*,#3479,.T.) ;
#5002 = ORIENTED_EDGE('',*,*,#3476,.T.) ;
#5003 = ORIENTED_EDGE('',*,*,#3473,.T.) ;
#5004 = ORIENTED_EDGE('',*,*,#3470,.T.) ;
#5005 = ORIENTED_EDGE('',*,*,#3467,.T.) ;
#5006 = ORIENTED_EDGE('',*,*,#3487,.F.) ;
#5007 = ORIENTED_EDGE('',*,*,#3465,.T.) ;
#5008 = ORIENTED_EDGE('',*,*,#3469,.F.) ;
#5009 = ORIENTED_EDGE('',*,*,#3472,.F.) ;
#5010 = ORIENTED_EDGE('',*,*,#3475,.T.) ;
#5011 = ORIENTED_EDGE('',*,*,#3478,.F.) ;
#5012 = ORIENTED_EDGE('',*,*,#3481,.F.) ;
#5013 = ORIENTED_EDGE('',*,*,#3484,.F.) ;
#5014 = ORIENTED_EDGE('',*,*,#3489,.F.) ;
#5015 = ORIENTED_EDGE('',*,*,#3490,.T.) ;
#5016 = ORIENTED_EDGE('',*,*,#3491,.T.) ;
#5017 = ORIENTED_EDGE('',*,*,#3490,.F.) ;
#5018 = ORIENTED_EDGE('',*,*,#3492,.F.) ;
#5019 = ORIENTED_EDGE('',*,*,#3493,.T.) ;
#5020 = ORIENTED_EDGE('',*,*,#3494,.F.) ;
#5021 = ORIENTED_EDGE('',*,*,#3495,.F.) ;
#5022 = ORIENTED_EDGE('',*,*,#3496,.T.) ;
#5023 = ORIENTED_EDGE('',*,*,#3495,.T.) ;
#5024 = ORIENTED_EDGE('',*,*,#3497,.F.) ;
#5025 = ORIENTED_EDGE('',*,*,#3498,.F.) ;
#5026 = ORIENTED_EDGE('',*,*,#3499,.T.) ;
#5027 = ORIENTED_EDGE('',*,*,#3498,.T.) ;
#5028 = ORIENTED_EDGE('',*,*,#3500,.F.) ;
#5029 = ORIENTED_EDGE('',*,*,#3501,.F.) ;
#5030 = ORIENTED_EDGE('',*,*,#3502,.T.) ;
#5031 = ORIENTED_EDGE('',*,*,#3501,.T.) ;
#5032 = ORIENTED_EDGE('',*,*,#3503,.F.) ;
#5033 = ORIENTED_EDGE('',*,*,#3504,.F.) ;
#5034 = ORIENTED_EDGE('',*,*,#3505,.T.) ;
#5035 = ORIENTED_EDGE('',*,*,#3504,.T.) ;
#5036 = ORIENTED_EDGE('',*,*,#3506,.F.) ;
#5037 = ORIENTED_EDGE('',*,*,#3507,.F.) ;
#5038 = ORIENTED_EDGE('',*,*,#3508,.T.) ;
#5039 = ORIENTED_EDGE('',*,*,#3507,.T.) ;
#5040 = ORIENTED_EDGE('',*,*,#3509,.F.) ;
#5041 = ORIENTED_EDGE('',*,*,#3510,.F.) ;
#5042 = ORIENTED_EDGE('',*,*,#3511,.T.) ;
#5043 = ORIENTED_EDGE('',*,*,#3510,.T.) ;
#5044 = ORIENTED_EDGE('',*,*,#3512,.F.) ;
#5045 = ORIENTED_EDGE('',*,*,#3513,.F.) ;
#5046 = ORIENTED_EDGE('',*,*,#3514,.T.) ;
#5047 = ORIENTED_EDGE('',*,*,#3513,.T.) ;
#5048 = ORIENTED_EDGE('',*,*,#3515,.F.) ;
#5049 = ORIENTED_EDGE('',*,*,#3516,.F.) ;
#5050 = ORIENTED_EDGE('',*,*,#3517,.T.) ;
#5051 = ORIENTED_EDGE('',*,*,#3516,.T.) ;
#5052 = ORIENTED_EDGE('',*,*,#3518,.F.) ;
#5053 = ORIENTED_EDGE('',*,*,#3519,.F.) ;
#5054 = ORIENTED_EDGE('',*,*,#3520,.T.) ;
#5055 = ORIENTED_EDGE('',*,*,#3519,.T.) ;
#5056 = ORIENTED_EDGE('',*,*,#3521,.F.) ;
#5057 = ORIENTED_EDGE('',*,*,#3493,.F.) ;
#5058 = ORIENTED_EDGE('',*,*,#3521,.T.) ;
#5059 = ORIENTED_EDGE('',*,*,#3518,.T.) ;
#5060 = ORIENTED_EDGE('',*,*,#3515,.T.) ;
#5061 = ORIENTED_EDGE('',*,*,#3512,.T.) ;
#5062 = ORIENTED_EDGE('',*,*,#3509,.T.) ;
#5063 = ORIENTED_EDGE('',*,*,#3506,.T.) ;
#5064 = ORIENTED_EDGE('',*,*,#3503,.T.) ;
#5065 = ORIENTED_EDGE('',*,*,#3500,.T.) ;
#5066 = ORIENTED_EDGE('',*,*,#3497,.T.) ;
#5067 = ORIENTED_EDGE('',*,*,#3494,.T.) ;
#5068 = ORIENTED_EDGE('',*,*,#3489,.T.) ;
#5069 = ORIENTED_EDGE('',*,*,#3520,.F.) ;
#5070 = ORIENTED_EDGE('',*,*,#3492,.T.) ;
#5071 = ORIENTED_EDGE('',*,*,#3496,.F.) ;
#5072 = ORIENTED_EDGE('',*,*,#3499,.F.) ;
#5073 = ORIENTED_EDGE('',*,*,#3502,.F.) ;
#5074 = ORIENTED_EDGE('',*,*,#3505,.F.) ;
#5075 = ORIENTED_EDGE('',*,*,#3508,.F.) ;
#5076 = ORIENTED_EDGE('',*,*,#3511,.F.) ;
#5077 = ORIENTED_EDGE('',*,*,#3514,.F.) ;
#5078 = ORIENTED_EDGE('',*,*,#3517,.F.) ;
#5079 = ORIENTED_EDGE('',*,*,#3491,.F.) ;
#5080 = ORIENTED_EDGE('',*,*,#3522,.T.) ;
#5081 = ORIENTED_EDGE('',*,*,#3523,.T.) ;
#5082 = ORIENTED_EDGE('',*,*,#3524,.F.) ;
#5083 = ORIENTED_EDGE('',*,*,#3523,.F.) ;
#5084 = ORIENTED_EDGE('',*,*,#3525,.F.) ;
#5085 = ORIENTED_EDGE('',*,*,#3524,.T.) ;
#5086 = ORIENTED_EDGE('',*,*,#3526,.F.) ;
#5087 = ORIENTED_EDGE('',*,*,#3527,.T.) ;
#5088 = ORIENTED_EDGE('',*,*,#3525,.T.) ;
#5089 = ORIENTED_EDGE('',*,*,#3527,.F.) ;
#5090 = ORIENTED_EDGE('',*,*,#3526,.T.) ;
#5091 = ORIENTED_EDGE('',*,*,#3522,.F.) ;
#5092 = CYLINDRICAL_SURFACE('',#5752,1.75) ;
#5093 = CYLINDRICAL_SURFACE('',#5755,3.98) ;
#5094 = CYLINDRICAL_SURFACE('',#5758,3.98) ;
#5095 = CYLINDRICAL_SURFACE('',#5771,3.175) ;
#5096 = CYLINDRICAL_SURFACE('',#5781,0.25) ;
#5097 = CYLINDRICAL_SURFACE('',#5787,0.25) ;
#5098 = CYLINDRICAL_SURFACE('',#5789,2.665) ;
#5099 = CYLINDRICAL_SURFACE('',#5799,2.665) ;
#5100 = CYLINDRICAL_SURFACE('',#5811,2.665) ;
#5101 = CYLINDRICAL_SURFACE('',#5817,0.25) ;
#5102 = CYLINDRICAL_SURFACE('',#5822,0.25) ;
#5103 = CYLINDRICAL_SURFACE('',#5824,2.665) ;
#5104 = CYLINDRICAL_SURFACE('',#5828,0.25) ;
#5105 = CYLINDRICAL_SURFACE('',#5830,0.25) ;
#5106 = CYLINDRICAL_SURFACE('',#5840,0.25) ;
#5107 = CYLINDRICAL_SURFACE('',#5852,0.25) ;
#5108 = CYLINDRICAL_SURFACE('',#5853,0.25) ;
#5109 = CYLINDRICAL_SURFACE('',#5855,0.25) ;
#5110 = CYLINDRICAL_SURFACE('',#5857,0.25) ;
#5111 = CYLINDRICAL_SURFACE('',#5864,0.25) ;
#5112 = CYLINDRICAL_SURFACE('',#5874,1.27) ;
#5113 = CYLINDRICAL_SURFACE('',#5877,1.27) ;
#5114 = CYLINDRICAL_SURFACE('',#5879,1.27) ;
#5115 = CYLINDRICAL_SURFACE('',#5882,3.175) ;
#5116 = CYLINDRICAL_SURFACE('',#5887,3.175) ;
#5117 = CYLINDRICAL_SURFACE('',#5888,3.175) ;
#5118 = CYLINDRICAL_SURFACE('',#5892,13.3598235398934) ;
#5119 = CYLINDRICAL_SURFACE('',#5895,3.22733975942849) ;
#5120 = CYLINDRICAL_SURFACE('',#5896,3.175) ;
#5121 = CYLINDRICAL_SURFACE('',#5898,3.175) ;
#5122 = CYLINDRICAL_SURFACE('',#5902,2.665) ;
#5123 = CYLINDRICAL_SURFACE('',#5905,2.665) ;
#5124 = CYLINDRICAL_SURFACE('',#5908,3.08595375255767) ;
#5125 = CYLINDRICAL_SURFACE('',#5911,16.5858074534161) ;
#5126 = CYLINDRICAL_SURFACE('',#5914,3.30499364382027) ;
#5127 = CYLINDRICAL_SURFACE('',#5917,0.249999999999995) ;
#5128 = CYLINDRICAL_SURFACE('',#5920,0.249999999999995) ;
#5129 = CYLINDRICAL_SURFACE('',#5924,0.25) ;
#5130 = CYLINDRICAL_SURFACE('',#5938,0.25) ;
#5131 = CYLINDRICAL_SURFACE('',#5949,0.25) ;
#5132 = CYLINDRICAL_SURFACE('',#5955,0.25) ;
#5133 = CYLINDRICAL_SURFACE('',#5957,2.665) ;
#5134 = CYLINDRICAL_SURFACE('',#5971,0.25) ;
#5135 = CYLINDRICAL_SURFACE('',#5976,0.25) ;
#5136 = CYLINDRICAL_SURFACE('',#5978,2.665) ;
#5137 = CYLINDRICAL_SURFACE('',#5980,0.25) ;
#5138 = CYLINDRICAL_SURFACE('',#5981,1.48867477559092) ;
#5139 = CYLINDRICAL_SURFACE('',#5984,0.25) ;
#5140 = CYLINDRICAL_SURFACE('',#5989,0.25) ;
#5141 = CYLINDRICAL_SURFACE('',#5995,0.25) ;
#5142 = CYLINDRICAL_SURFACE('',#6000,0.25) ;
#5143 = CYLINDRICAL_SURFACE('',#6002,0.649999999999999) ;
#5144 = CYLINDRICAL_SURFACE('',#6005,6.20626157119473) ;
#5145 = CYLINDRICAL_SURFACE('',#6007,47.1073015873016) ;
#5146 = CYLINDRICAL_SURFACE('',#6009,6.4566222212067) ;
#5147 = CYLINDRICAL_SURFACE('',#6012,0.650000000000004) ;
#5148 = CYLINDRICAL_SURFACE('',#6015,1.585) ;
#5149 = CYLINDRICAL_SURFACE('',#6017,1.585) ;
#5150 = CYLINDRICAL_SURFACE('',#6024,5.45) ;
#5151 = CYLINDRICAL_SURFACE('',#6033,5.66550083849775) ;
#5152 = CYLINDRICAL_SURFACE('',#6035,2.665) ;
#5153 = CYLINDRICAL_SURFACE('',#6037,2.665) ;
#5154 = CYLINDRICAL_SURFACE('',#6039,0.2) ;
#5155 = CYLINDRICAL_SURFACE('',#6042,0.2) ;
#5156 = CYLINDRICAL_SURFACE('',#6046,0.2) ;
#5157 = CYLINDRICAL_SURFACE('',#6050,0.2) ;
#5158 = CYLINDRICAL_SURFACE('',#6054,0.2) ;
#5159 = CYLINDRICAL_SURFACE('',#6058,0.2) ;
#5160 = CYLINDRICAL_SURFACE('',#6059,0.2) ;
#5161 = CYLINDRICAL_SURFACE('',#6074,0.2) ;
#5162 = CYLINDRICAL_SURFACE('',#6075,0.2) ;
#5163 = CYLINDRICAL_SURFACE('',#6076,0.2) ;
#5164 = CYLINDRICAL_SURFACE('',#6083,0.2) ;
#5165 = CYLINDRICAL_SURFACE('',#6088,0.2) ;
#5166 = CYLINDRICAL_SURFACE('',#6092,0.2) ;
#5167 = CYLINDRICAL_SURFACE('',#6096,0.2) ;
#5168 = CYLINDRICAL_SURFACE('',#6100,0.474381812079108) ;
#5169 = CYLINDRICAL_SURFACE('',#6103,0.332505429325631) ;
#5170 = CYLINDRICAL_SURFACE('',#6106,5.4095419988581) ;
#5171 = CYLINDRICAL_SURFACE('',#6109,6.22789861439302) ;
#5172 = CYLINDRICAL_SURFACE('',#6111,0.324935224963979) ;
#5173 = CYLINDRICAL_SURFACE('',#6114,1.20004201680672) ;
#5174 = CYLINDRICAL_SURFACE('',#6117,1.6962519345458) ;
#5175 = CYLINDRICAL_SURFACE('',#6119,6.44675996480777) ;
#5176 = CYLINDRICAL_SURFACE('',#6122,9.57267576253889) ;
#5177 = CYLINDRICAL_SURFACE('',#6130,0.2) ;
#5178 = CYLINDRICAL_SURFACE('',#6134,0.2) ;
#5179 = CYLINDRICAL_SURFACE('',#6138,0.2) ;
#5180 = CYLINDRICAL_SURFACE('',#6143,0.2) ;
#5181 = CYLINDRICAL_SURFACE('',#6149,0.2) ;
#5182 = CYLINDRICAL_SURFACE('',#6154,0.2) ;
#5183 = CYLINDRICAL_SURFACE('',#6155,0.2) ;
#5184 = CYLINDRICAL_SURFACE('',#6161,0.2) ;
#5185 = CYLINDRICAL_SURFACE('',#6164,0.2) ;
#5186 = CYLINDRICAL_SURFACE('',#6165,0.2) ;
#5187 = CYLINDRICAL_SURFACE('',#6168,0.2) ;
#5188 = CYLINDRICAL_SURFACE('',#6174,0.2) ;
#5189 = CYLINDRICAL_SURFACE('',#6177,0.2) ;
#5190 = CYLINDRICAL_SURFACE('',#6179,0.2) ;
#5191 = CYLINDRICAL_SURFACE('',#6181,4.17909654020415) ;
#5192 = CYLINDRICAL_SURFACE('',#6183,3.76067266925812) ;
#5193 = CYLINDRICAL_SURFACE('',#6185,18.9717409779691) ;
#5194 = CYLINDRICAL_SURFACE('',#6187,7.93937148944777) ;
#5195 = CYLINDRICAL_SURFACE('',#6189,4.43606098801213) ;
#5196 = CYLINDRICAL_SURFACE('',#6192,20.767808830506) ;
#5197 = CYLINDRICAL_SURFACE('',#6198,0.2) ;
#5198 = CYLINDRICAL_SURFACE('',#6201,0.2) ;
#5199 = CYLINDRICAL_SURFACE('',#6204,0.65017716535433) ;
#5200 = CYLINDRICAL_SURFACE('',#6210,0.2) ;
#5201 = CYLINDRICAL_SURFACE('',#6211,0.2) ;
#5202 = CYLINDRICAL_SURFACE('',#6212,3.97) ;
#5203 = CYLINDRICAL_SURFACE('',#6214,0.65017716535433) ;
#5204 = CYLINDRICAL_SURFACE('',#6220,3.95) ;
#5205 = CYLINDRICAL_SURFACE('',#6228,1.5) ;
#5206 = CYLINDRICAL_SURFACE('',#6234,5.175) ;
#5207 = CYLINDRICAL_SURFACE('',#6240,1.5) ;
#5208 = CYLINDRICAL_SURFACE('',#6248,1.65) ;
#5209 = CYLINDRICAL_SURFACE('',#6254,1.7) ;
#5210 = CYLINDRICAL_SURFACE('',#6280,1.90519525249383) ;
#5211 = CYLINDRICAL_SURFACE('',#6284,1.62016604149081) ;
#5212 = CYLINDRICAL_SURFACE('',#6290,0.605) ;
#5213 = CYLINDRICAL_SURFACE('',#6302,0.605) ;
#5214 = CYLINDRICAL_SURFACE('',#6312,3.985) ;
#5215 = CYLINDRICAL_SURFACE('',#6317,6.105) ;
#5216 = CYLINDRICAL_SURFACE('',#6321,3.985) ;
#5217 = CYLINDRICAL_SURFACE('',#6326,5.4) ;
#5218 = CYLINDRICAL_SURFACE('',#6330,3.985) ;
#5219 = CYLINDRICAL_SURFACE('',#6335,5.595) ;
#5220 = CYLINDRICAL_SURFACE('',#6339,2.55000000000001) ;
#5221 = CYLINDRICAL_SURFACE('',#6344,4.00044834860818) ;
#5222 = CYLINDRICAL_SURFACE('',#6348,13.4930018479188) ;
#5223 = CYLINDRICAL_SURFACE('',#6351,1.26348906976575) ;
#5224 = CYLINDRICAL_SURFACE('',#6358,3.97) ;
#5225 = CYLINDRICAL_SURFACE('',#6361,2.55000000000001) ;
#5226 = CYLINDRICAL_SURFACE('',#6365,1.34638068543699) ;
#5227 = CYLINDRICAL_SURFACE('',#6368,13.5130476224576) ;
#5228 = CYLINDRICAL_SURFACE('',#6372,1.8820937834387) ;
#5229 = CYLINDRICAL_SURFACE('',#6376,13.5002427920346) ;
#5230 = CYLINDRICAL_SURFACE('',#6379,1.26348906976575) ;
#5231 = CYLINDRICAL_SURFACE('',#6386,1.525) ;
#5232 = CYLINDRICAL_SURFACE('',#6391,2.225) ;
#5233 = ADVANCED_FACE('',(#508),#5092,.F.) ;
#5234 = ADVANCED_FACE('',(#509),#5093,.F.) ;
#5235 = ADVANCED_FACE('',(#510),#5094,.F.) ;
#5236 = ADVANCED_FACE('',(#511),#396,.F.) ;
#5237 = ADVANCED_FACE('',(#512,#337),#397,.F.) ;
#5238 = ADVANCED_FACE('',(#513),#398,.F.) ;
#5239 = ADVANCED_FACE('',(#514),#399,.F.) ;
#5240 = ADVANCED_FACE('',(#515,#338),#400,.F.) ;
#5241 = ADVANCED_FACE('',(#516),#401,.F.) ;
#5242 = ADVANCED_FACE('',(#517,#339),#402,.T.) ;
#5243 = ADVANCED_FACE('',(#518),#403,.T.) ;
#5244 = ADVANCED_FACE('',(#519),#5095,.T.) ;
#5245 = ADVANCED_FACE('',(#520),#404,.T.) ;
#5246 = ADVANCED_FACE('',(#521),#176,.T.) ;
#5247 = ADVANCED_FACE('',(#522),#5096,.T.) ;
#5248 = ADVANCED_FACE('',(#523),#177,.T.) ;
#5249 = ADVANCED_FACE('',(#524),#5097,.T.) ;
#5250 = ADVANCED_FACE('',(#525),#405,.T.) ;
#5251 = ADVANCED_FACE('',(#526),#5098,.F.) ;
#5252 = ADVANCED_FACE('',(#527,#340,#341),#406,.T.) ;
#5253 = ADVANCED_FACE('',(#528),#178,.T.) ;
#5254 = ADVANCED_FACE('',(#529),#5099,.F.) ;
#5255 = ADVANCED_FACE('',(#530),#179,.T.) ;
#5256 = ADVANCED_FACE('',(#531,#342,#343),#407,.T.) ;
#5257 = ADVANCED_FACE('',(#532),#5100,.F.) ;
#5258 = ADVANCED_FACE('',(#533),#180,.T.) ;
#5259 = ADVANCED_FACE('',(#534),#5101,.T.) ;
#5260 = ADVANCED_FACE('',(#535),#181,.T.) ;
#5261 = ADVANCED_FACE('',(#536),#5102,.T.) ;
#5262 = ADVANCED_FACE('',(#537),#408,.T.) ;
#5263 = ADVANCED_FACE('',(#538),#5103,.F.) ;
#5264 = ADVANCED_FACE('',(#539),#170,.F.) ;
#5265 = ADVANCED_FACE('',(#540),#5104,.T.) ;
#5266 = ADVANCED_FACE('',(#541),#5105,.T.) ;
#5267 = ADVANCED_FACE('',(#542),#182,.T.) ;
#5268 = ADVANCED_FACE('',(#543),#183,.T.) ;
#5269 = ADVANCED_FACE('',(#544),#184,.T.) ;
#5270 = ADVANCED_FACE('',(#545),#5106,.T.) ;
#5271 = ADVANCED_FACE('',(#546),#171,.F.) ;
#5272 = ADVANCED_FACE('',(#547),#172,.F.) ;
#5273 = ADVANCED_FACE('',(#548),#185,.T.) ;
#5274 = ADVANCED_FACE('',(#549),#173,.F.) ;
#5275 = ADVANCED_FACE('',(#550),#186,.T.) ;
#5276 = ADVANCED_FACE('',(#551),#174,.F.) ;
#5277 = ADVANCED_FACE('',(#552),#187,.T.) ;
#5278 = ADVANCED_FACE('',(#553),#5107,.T.) ;
#5279 = ADVANCED_FACE('',(#554),#5108,.T.) ;
#5280 = ADVANCED_FACE('',(#555),#5109,.T.) ;
#5281 = ADVANCED_FACE('',(#556),#5110,.T.) ;
#5282 = ADVANCED_FACE('',(#557),#188,.T.) ;
#5283 = ADVANCED_FACE('',(#558),#5111,.T.) ;
#5284 = ADVANCED_FACE('',(#559),#175,.F.) ;
#5285 = ADVANCED_FACE('',(#560),#168,.T.) ;
#5286 = ADVANCED_FACE('',(#561),#169,.T.) ;
#5287 = ADVANCED_FACE('',(#562,#344),#409,.T.) ;
#5288 = ADVANCED_FACE('',(#563),#5112,.F.) ;
#5289 = ADVANCED_FACE('',(#564),#410,.T.) ;
#5290 = ADVANCED_FACE('',(#565),#5113,.F.) ;
#5291 = ADVANCED_FACE('',(#566),#5114,.F.) ;
#5292 = ADVANCED_FACE('',(#567,#345),#411,.F.) ;
#5293 = ADVANCED_FACE('',(#568),#5115,.T.) ;
#5294 = ADVANCED_FACE('',(#569),#189,.T.) ;
#5295 = ADVANCED_FACE('',(#570),#5116,.T.) ;
#5296 = ADVANCED_FACE('',(#571),#5117,.T.) ;
#5297 = ADVANCED_FACE('',(#572),#412,.T.) ;
#5298 = ADVANCED_FACE('',(#573),#413,.T.) ;
#5299 = ADVANCED_FACE('',(#574),#5118,.T.) ;
#5300 = ADVANCED_FACE('',(#575),#414,.T.) ;
#5301 = ADVANCED_FACE('',(#576),#5119,.T.) ;
#5302 = ADVANCED_FACE('',(#577),#5120,.T.) ;
#5303 = ADVANCED_FACE('',(#578),#5121,.T.) ;
#5304 = ADVANCED_FACE('',(#579),#190,.T.) ;
#5305 = ADVANCED_FACE('',(#580,#346),#415,.T.) ;
#5306 = ADVANCED_FACE('',(#581),#416,.T.) ;
#5307 = ADVANCED_FACE('',(#582),#5122,.F.) ;
#5308 = ADVANCED_FACE('',(#583),#417,.T.) ;
#5309 = ADVANCED_FACE('',(#584),#5123,.F.) ;
#5310 = ADVANCED_FACE('',(#585),#418,.T.) ;
#5311 = ADVANCED_FACE('',(#586),#5124,.T.) ;
#5312 = ADVANCED_FACE('',(#587),#419,.T.) ;
#5313 = ADVANCED_FACE('',(#588),#5125,.T.) ;
#5314 = ADVANCED_FACE('',(#589),#420,.T.) ;
#5315 = ADVANCED_FACE('',(#590),#5126,.T.) ;
#5316 = ADVANCED_FACE('',(#591),#421,.T.) ;
#5317 = ADVANCED_FACE('',(#592),#5127,.T.) ;
#5318 = ADVANCED_FACE('',(#593),#422,.T.) ;
#5319 = ADVANCED_FACE('',(#594),#5128,.T.) ;
#5320 = ADVANCED_FACE('',(#595,#347,#348,#349,#350),#423,.F.) ;
#5321 = ADVANCED_FACE('',(#596),#5129,.F.) ;
#5322 = ADVANCED_FACE('',(#597),#191,.F.) ;
#5323 = ADVANCED_FACE('',(#598,#351),#424,.F.) ;
#5324 = ADVANCED_FACE('',(#599),#192,.F.) ;
#5325 = ADVANCED_FACE('',(#600),#5130,.F.) ;
#5326 = ADVANCED_FACE('',(#601,#352),#425,.T.) ;
#5327 = ADVANCED_FACE('',(#602),#193,.T.) ;
#5328 = ADVANCED_FACE('',(#603),#5131,.T.) ;
#5329 = ADVANCED_FACE('',(#604),#194,.T.) ;
#5330 = ADVANCED_FACE('',(#605),#5132,.T.) ;
#5331 = ADVANCED_FACE('',(#606),#426,.T.) ;
#5332 = ADVANCED_FACE('',(#607),#5133,.F.) ;
#5333 = ADVANCED_FACE('',(#608,#353,#354),#427,.T.) ;
#5334 = ADVANCED_FACE('',(#609),#195,.T.) ;
#5335 = ADVANCED_FACE('',(#610),#5134,.T.) ;
#5336 = ADVANCED_FACE('',(#611),#196,.T.) ;
#5337 = ADVANCED_FACE('',(#612),#5135,.T.) ;
#5338 = ADVANCED_FACE('',(#613),#428,.T.) ;
#5339 = ADVANCED_FACE('',(#614),#5136,.F.) ;
#5340 = ADVANCED_FACE('',(#615),#5137,.F.) ;
#5341 = ADVANCED_FACE('',(#616),#5138,.F.) ;
#5342 = ADVANCED_FACE('',(#617),#197,.T.) ;
#5343 = ADVANCED_FACE('',(#618),#5139,.T.) ;
#5344 = ADVANCED_FACE('',(#619),#198,.T.) ;
#5345 = ADVANCED_FACE('',(#620),#5140,.T.) ;
#5346 = ADVANCED_FACE('',(#621),#199,.T.) ;
#5347 = ADVANCED_FACE('',(#622),#200,.T.) ;
#5348 = ADVANCED_FACE('',(#623),#5141,.T.) ;
#5349 = ADVANCED_FACE('',(#624),#201,.T.) ;
#5350 = ADVANCED_FACE('',(#625),#5142,.T.) ;
#5351 = ADVANCED_FACE('',(#626),#429,.T.) ;
#5352 = ADVANCED_FACE('',(#627),#5143,.T.) ;
#5353 = ADVANCED_FACE('',(#628),#430,.T.) ;
#5354 = ADVANCED_FACE('',(#629),#5144,.T.) ;
#5355 = ADVANCED_FACE('',(#630),#5145,.T.) ;
#5356 = ADVANCED_FACE('',(#631),#5146,.T.) ;
#5357 = ADVANCED_FACE('',(#632),#431,.T.) ;
#5358 = ADVANCED_FACE('',(#633),#5147,.T.) ;
#5359 = ADVANCED_FACE('',(#634),#432,.T.) ;
#5360 = ADVANCED_FACE('',(#635),#5148,.F.) ;
#5361 = ADVANCED_FACE('',(#636),#5149,.F.) ;
#5362 = ADVANCED_FACE('',(#637,#355),#433,.F.) ;
#5363 = ADVANCED_FACE('',(#638),#434,.F.) ;
#5364 = ADVANCED_FACE('',(#639),#435,.F.) ;
#5365 = ADVANCED_FACE('',(#640),#5150,.F.) ;
#5366 = ADVANCED_FACE('',(#641),#436,.F.) ;
#5367 = ADVANCED_FACE('',(#642,#356),#437,.T.) ;
#5368 = ADVANCED_FACE('',(#643,#357,#358),#438,.F.) ;
#5369 = ADVANCED_FACE('',(#644),#439,.T.) ;
#5370 = ADVANCED_FACE('',(#645),#5151,.T.) ;
#5371 = ADVANCED_FACE('',(#646),#440,.T.) ;
#5372 = ADVANCED_FACE('',(#647),#5152,.F.) ;
#5373 = ADVANCED_FACE('',(#648),#441,.T.) ;
#5374 = ADVANCED_FACE('',(#649),#5153,.F.) ;
#5375 = ADVANCED_FACE('',(#650),#5154,.T.) ;
#5376 = ADVANCED_FACE('',(#651),#106,.F.) ;
#5377 = ADVANCED_FACE('',(#652),#5155,.T.) ;
#5378 = ADVANCED_FACE('',(#653),#202,.T.) ;
#5379 = ADVANCED_FACE('',(#654),#5156,.T.) ;
#5380 = ADVANCED_FACE('',(#655),#203,.T.) ;
#5381 = ADVANCED_FACE('',(#656),#5157,.T.) ;
#5382 = ADVANCED_FACE('',(#657),#204,.T.) ;
#5383 = ADVANCED_FACE('',(#658),#5158,.T.) ;
#5384 = ADVANCED_FACE('',(#659),#205,.T.) ;
#5385 = ADVANCED_FACE('',(#660),#5159,.T.) ;
#5386 = ADVANCED_FACE('',(#661),#5160,.T.) ;
#5387 = ADVANCED_FACE('',(#662),#206,.T.) ;
#5388 = ADVANCED_FACE('',(#663),#207,.T.) ;
#5389 = ADVANCED_FACE('',(#664),#208,.T.) ;
#5390 = ADVANCED_FACE('',(#665),#209,.T.) ;
#5391 = ADVANCED_FACE('',(#666),#5161,.T.) ;
#5392 = ADVANCED_FACE('',(#667),#5162,.T.) ;
#5393 = ADVANCED_FACE('',(#668),#5163,.T.) ;
#5394 = ADVANCED_FACE('',(#669),#210,.T.) ;
#5395 = ADVANCED_FACE('',(#670),#211,.T.) ;
#5396 = ADVANCED_FACE('',(#671),#5164,.T.) ;
#5397 = ADVANCED_FACE('',(#672),#212,.T.) ;
#5398 = ADVANCED_FACE('',(#673),#5165,.T.) ;
#5399 = ADVANCED_FACE('',(#674),#213,.T.) ;
#5400 = ADVANCED_FACE('',(#675),#5166,.T.) ;
#5401 = ADVANCED_FACE('',(#676),#214,.T.) ;
#5402 = ADVANCED_FACE('',(#677),#5167,.T.) ;
#5403 = ADVANCED_FACE('',(#678),#215,.T.) ;
#5404 = ADVANCED_FACE('',(#679),#5168,.T.) ;
#5405 = ADVANCED_FACE('',(#680),#442,.T.) ;
#5406 = ADVANCED_FACE('',(#681),#5169,.T.) ;
#5407 = ADVANCED_FACE('',(#682),#443,.T.) ;
#5408 = ADVANCED_FACE('',(#683),#5170,.F.) ;
#5409 = ADVANCED_FACE('',(#684),#444,.T.) ;
#5410 = ADVANCED_FACE('',(#685),#5171,.T.) ;
#5411 = ADVANCED_FACE('',(#686),#5172,.F.) ;
#5412 = ADVANCED_FACE('',(#687),#445,.T.) ;
#5413 = ADVANCED_FACE('',(#688),#5173,.T.) ;
#5414 = ADVANCED_FACE('',(#689),#446,.T.) ;
#5415 = ADVANCED_FACE('',(#690),#5174,.F.) ;
#5416 = ADVANCED_FACE('',(#691),#5175,.T.) ;
#5417 = ADVANCED_FACE('',(#692),#447,.T.) ;
#5418 = ADVANCED_FACE('',(#693),#5176,.F.) ;
#5419 = ADVANCED_FACE('',(#694,#359,#360),#448,.T.) ;
#5420 = ADVANCED_FACE('',(#695),#216,.T.) ;
#5421 = ADVANCED_FACE('',(#696),#5177,.T.) ;
#5422 = ADVANCED_FACE('',(#697),#217,.T.) ;
#5423 = ADVANCED_FACE('',(#698),#5178,.T.) ;
#5424 = ADVANCED_FACE('',(#699),#218,.T.) ;
#5425 = ADVANCED_FACE('',(#700),#5179,.T.) ;
#5426 = ADVANCED_FACE('',(#701),#219,.T.) ;
#5427 = ADVANCED_FACE('',(#702),#5180,.T.) ;
#5428 = ADVANCED_FACE('',(#703),#220,.T.) ;
#5429 = ADVANCED_FACE('',(#704),#221,.T.) ;
#5430 = ADVANCED_FACE('',(#705),#5181,.T.) ;
#5431 = ADVANCED_FACE('',(#706),#222,.T.) ;
#5432 = ADVANCED_FACE('',(#707),#5182,.T.) ;
#5433 = ADVANCED_FACE('',(#708),#5183,.T.) ;
#5434 = ADVANCED_FACE('',(#709),#223,.T.) ;
#5435 = ADVANCED_FACE('',(#710),#224,.T.) ;
#5436 = ADVANCED_FACE('',(#711),#5184,.T.) ;
#5437 = ADVANCED_FACE('',(#712),#225,.T.) ;
#5438 = ADVANCED_FACE('',(#713),#5185,.T.) ;
#5439 = ADVANCED_FACE('',(#714),#5186,.T.) ;
#5440 = ADVANCED_FACE('',(#715),#226,.T.) ;
#5441 = ADVANCED_FACE('',(#716),#5187,.T.) ;
#5442 = ADVANCED_FACE('',(#717),#227,.T.) ;
#5443 = ADVANCED_FACE('',(#718),#228,.T.) ;
#5444 = ADVANCED_FACE('',(#719),#5188,.T.) ;
#5445 = ADVANCED_FACE('',(#720),#229,.T.) ;
#5446 = ADVANCED_FACE('',(#721),#5189,.T.) ;
#5447 = ADVANCED_FACE('',(#722),#107,.F.) ;
#5448 = ADVANCED_FACE('',(#723),#5190,.T.) ;
#5449 = ADVANCED_FACE('',(#724),#449,.T.) ;
#5450 = ADVANCED_FACE('',(#725),#5191,.F.) ;
#5451 = ADVANCED_FACE('',(#726),#450,.T.) ;
#5452 = ADVANCED_FACE('',(#727),#5192,.F.) ;
#5453 = ADVANCED_FACE('',(#728),#451,.T.) ;
#5454 = ADVANCED_FACE('',(#729),#5193,.T.) ;
#5455 = ADVANCED_FACE('',(#730),#452,.T.) ;
#5456 = ADVANCED_FACE('',(#731),#5194,.F.) ;
#5457 = ADVANCED_FACE('',(#732),#453,.T.) ;
#5458 = ADVANCED_FACE('',(#733),#5195,.T.) ;
#5459 = ADVANCED_FACE('',(#734),#454,.T.) ;
#5460 = ADVANCED_FACE('',(#735),#455,.T.) ;
#5461 = ADVANCED_FACE('',(#736),#5196,.T.) ;
#5462 = ADVANCED_FACE('',(#737),#456,.T.) ;
#5463 = ADVANCED_FACE('',(#738,#361,#362),#457,.F.) ;
#5464 = ADVANCED_FACE('',(#739),#5197,.T.) ;
#5465 = ADVANCED_FACE('',(#740),#230,.T.) ;
#5466 = ADVANCED_FACE('',(#741),#5198,.T.) ;
#5467 = ADVANCED_FACE('',(#742),#231,.T.) ;
#5468 = ADVANCED_FACE('',(#743),#5199,.F.) ;
#5469 = ADVANCED_FACE('',(#744),#458,.T.) ;
#5470 = ADVANCED_FACE('',(#745),#232,.T.) ;
#5471 = ADVANCED_FACE('',(#746),#233,.T.) ;
#5472 = ADVANCED_FACE('',(#747),#5200,.T.) ;
#5473 = ADVANCED_FACE('',(#748),#5201,.T.) ;
#5474 = ADVANCED_FACE('',(#749),#5202,.F.) ;
#5475 = ADVANCED_FACE('',(#750),#459,.T.) ;
#5476 = ADVANCED_FACE('',(#751),#5203,.F.) ;
#5477 = ADVANCED_FACE('',(#752),#460,.T.) ;
#5478 = ADVANCED_FACE('',(#753),#95,.T.) ;
#5479 = ADVANCED_FACE('',(#754),#5204,.T.) ;
#5480 = ADVANCED_FACE('',(#755),#96,.T.) ;
#5481 = ADVANCED_FACE('',(#756),#461,.T.) ;
#5482 = ADVANCED_FACE('',(#757),#462,.T.) ;
#5483 = ADVANCED_FACE('',(#758),#5205,.T.) ;
#5484 = ADVANCED_FACE('',(#759,#363),#463,.T.) ;
#5485 = ADVANCED_FACE('',(#760),#97,.T.) ;
#5486 = ADVANCED_FACE('',(#761),#5206,.T.) ;
#5487 = ADVANCED_FACE('',(#762),#98,.T.) ;
#5488 = ADVANCED_FACE('',(#763,#364),#464,.T.) ;
#5489 = ADVANCED_FACE('',(#764),#5207,.T.) ;
#5490 = ADVANCED_FACE('',(#765),#465,.T.) ;
#5491 = ADVANCED_FACE('',(#766),#466,.T.) ;
#5492 = ADVANCED_FACE('',(#767),#99,.T.) ;
#5493 = ADVANCED_FACE('',(#768),#5208,.T.) ;
#5494 = ADVANCED_FACE('',(#769),#100,.T.) ;
#5495 = ADVANCED_FACE('',(#770),#467,.T.) ;
#5496 = ADVANCED_FACE('',(#771),#5209,.F.) ;
#5497 = ADVANCED_FACE('',(#772),#468,.T.) ;
#5498 = ADVANCED_FACE('',(#773),#469,.T.) ;
#5499 = ADVANCED_FACE('',(#774),#470,.T.) ;
#5500 = ADVANCED_FACE('',(#775),#471,.T.) ;
#5501 = ADVANCED_FACE('',(#776),#472,.T.) ;
#5502 = ADVANCED_FACE('',(#777),#473,.T.) ;
#5503 = ADVANCED_FACE('',(#778),#474,.T.) ;
#5504 = ADVANCED_FACE('',(#779),#475,.T.) ;
#5505 = ADVANCED_FACE('',(#780),#476,.T.) ;
#5506 = ADVANCED_FACE('',(#781,#365),#477,.T.) ;
#5507 = ADVANCED_FACE('',(#782,#366),#478,.F.) ;
#5508 = ADVANCED_FACE('',(#783),#479,.F.) ;
#5509 = ADVANCED_FACE('',(#784),#480,.F.) ;
#5510 = ADVANCED_FACE('',(#785),#481,.F.) ;
#5511 = ADVANCED_FACE('',(#786),#482,.F.) ;
#5512 = ADVANCED_FACE('',(#787),#483,.F.) ;
#5513 = ADVANCED_FACE('',(#788),#484,.F.) ;
#5514 = ADVANCED_FACE('',(#789),#485,.F.) ;
#5515 = ADVANCED_FACE('',(#790,#367),#486,.T.) ;
#5516 = ADVANCED_FACE('',(#791),#101,.T.) ;
#5517 = ADVANCED_FACE('',(#792),#5210,.T.) ;
#5518 = ADVANCED_FACE('',(#793),#102,.T.) ;
#5519 = ADVANCED_FACE('',(#794),#5211,.T.) ;
#5520 = ADVANCED_FACE('',(#795),#103,.T.) ;
#5521 = ADVANCED_FACE('',(#796),#487,.T.) ;
#5522 = ADVANCED_FACE('',(#797),#5212,.T.) ;
#5523 = ADVANCED_FACE('',(#798),#104,.T.) ;
#5524 = ADVANCED_FACE('',(#799),#234,.T.) ;
#5525 = ADVANCED_FACE('',(#800),#235,.T.) ;
#5526 = ADVANCED_FACE('',(#801),#5213,.T.) ;
#5527 = ADVANCED_FACE('',(#802),#105,.T.) ;
#5528 = ADVANCED_FACE('',(#803),#236,.T.) ;
#5529 = ADVANCED_FACE('',(#804),#237,.T.) ;
#5530 = ADVANCED_FACE('',(#805),#5214,.F.) ;
#5531 = ADVANCED_FACE('',(#806,#368),#488,.T.) ;
#5532 = ADVANCED_FACE('',(#807),#5215,.T.) ;
#5533 = ADVANCED_FACE('',(#808,#369),#489,.T.) ;
#5534 = ADVANCED_FACE('',(#809),#5216,.F.) ;
#5535 = ADVANCED_FACE('',(#810,#370),#490,.T.) ;
#5536 = ADVANCED_FACE('',(#811),#5217,.T.) ;
#5537 = ADVANCED_FACE('',(#812,#371),#491,.T.) ;
#5538 = ADVANCED_FACE('',(#813),#5218,.F.) ;
#5539 = ADVANCED_FACE('',(#814,#372),#492,.T.) ;
#5540 = ADVANCED_FACE('',(#815),#5219,.T.) ;
#5541 = ADVANCED_FACE('',(#816,#373),#493,.T.) ;
#5542 = ADVANCED_FACE('',(#817),#5220,.F.) ;
#5543 = ADVANCED_FACE('',(#818),#494,.T.) ;
#5544 = ADVANCED_FACE('',(#819),#495,.T.) ;
#5545 = ADVANCED_FACE('',(#820),#5221,.F.) ;
#5546 = ADVANCED_FACE('',(#821),#496,.T.) ;
#5547 = ADVANCED_FACE('',(#822),#5222,.T.) ;
#5548 = ADVANCED_FACE('',(#823),#5223,.T.) ;
#5549 = ADVANCED_FACE('',(#824),#497,.T.) ;
#5550 = ADVANCED_FACE('',(#825),#498,.T.) ;
#5551 = ADVANCED_FACE('',(#826),#499,.F.) ;
#5552 = ADVANCED_FACE('',(#827),#5224,.F.) ;
#5553 = ADVANCED_FACE('',(#828),#5225,.F.) ;
#5554 = ADVANCED_FACE('',(#829),#500,.T.) ;
#5555 = ADVANCED_FACE('',(#830),#5226,.T.) ;
#5556 = ADVANCED_FACE('',(#831),#5227,.T.) ;
#5557 = ADVANCED_FACE('',(#832),#501,.T.) ;
#5558 = ADVANCED_FACE('',(#833),#5228,.T.) ;
#5559 = ADVANCED_FACE('',(#834),#502,.T.) ;
#5560 = ADVANCED_FACE('',(#835),#5229,.T.) ;
#5561 = ADVANCED_FACE('',(#836),#5230,.T.) ;
#5562 = ADVANCED_FACE('',(#837),#503,.T.) ;
#5563 = ADVANCED_FACE('',(#838,#374),#504,.T.) ;
#5564 = ADVANCED_FACE('',(#839,#375),#505,.F.) ;
#5565 = ADVANCED_FACE('',(#840),#5231,.F.) ;
#5566 = ADVANCED_FACE('',(#841,#376),#506,.T.) ;
#5567 = ADVANCED_FACE('',(#842),#5232,.T.) ;
#5568 = ADVANCED_FACE('',(#843,#377),#507,.T.) ;
#5569 = CLOSED_SHELL('',(#5233,#5234,#5235,#5236,#5237,#5238,#5239,#5240,
#5241,#5242,#5243,#5244,#5245,#5246,#5247,#5248,#5249,#5250,#5251,#5252,
#5253,#5254,#5255,#5256,#5257,#5258,#5259,#5260,#5261,#5262,#5263,#5264,
#5265,#5266,#5267,#5268,#5269,#5270,#5271,#5272,#5273,#5274,#5275,#5276,
#5277,#5278,#5279,#5280,#5281,#5282,#5283,#5284,#5285,#5286,#5287,#5288,
#5289,#5290,#5291,#5292,#5293,#5294,#5295,#5296,#5297,#5298,#5299,#5300,
#5301,#5302,#5303,#5304,#5305,#5306,#5307,#5308,#5309,#5310,#5311,#5312,
#5313,#5314,#5315,#5316,#5317,#5318,#5319,#5320)) ;
#5570 = CLOSED_SHELL('',(#5321,#5322,#5323,#5324,#5325,#5326,#5327,#5328,
#5329,#5330,#5331,#5332,#5333,#5334,#5335,#5336,#5337,#5338,#5339,#5340,
#5341,#5342,#5343,#5344,#5345,#5346,#5347,#5348,#5349,#5350,#5351,#5352,
#5353,#5354,#5355,#5356,#5357,#5358,#5359,#5360,#5361,#5362,#5363,#5364,
#5365,#5366,#5367,#5368,#5369,#5370,#5371,#5372,#5373,#5374)) ;
#5571 = CLOSED_SHELL('',(#5375,#5376,#5377,#5378,#5379,#5380,#5381,#5382,
#5383,#5384,#5385,#5386,#5387,#5388,#5389,#5390,#5391,#5392,#5393,#5394,
#5395,#5396,#5397,#5398,#5399,#5400,#5401,#5402,#5403,#5404,#5405,#5406,
#5407,#5408,#5409,#5410,#5411,#5412,#5413,#5414,#5415,#5416,#5417,#5418,
#5419,#5420,#5421,#5422,#5423,#5424,#5425,#5426,#5427,#5428,#5429,#5430,
#5431,#5432,#5433,#5434,#5435,#5436,#5437,#5438,#5439,#5440,#5441,#5442,
#5443,#5444,#5445,#5446,#5447,#5448,#5449,#5450,#5451,#5452,#5453,#5454,
#5455,#5456,#5457,#5458,#5459,#5460,#5461,#5462,#5463,#5464,#5465,#5466,
#5467,#5468,#5469,#5470,#5471,#5472,#5473,#5474,#5475,#5476)) ;
#5572 = CLOSED_SHELL('',(#5477,#5478,#5479,#5480,#5481)) ;
#5573 = CLOSED_SHELL('',(#5482,#5483,#5484,#5485,#5486,#5487,#5488,#5489,
#5490)) ;
#5574 = CLOSED_SHELL('',(#5491,#5492,#5493,#5494,#5495)) ;
#5575 = CLOSED_SHELL('',(#5496,#5497,#5498,#5499,#5500,#5501,#5502,#5503,
#5504,#5505,#5506,#5507)) ;
#5576 = CLOSED_SHELL('',(#5508,#5509,#5510,#5511,#5512,#5513,#5514,#5515,
#5516,#5517,#5518,#5519,#5520,#5521)) ;
#5577 = CLOSED_SHELL('',(#5522,#5523,#5524,#5525,#5526,#5527,#5528,#5529)) ;
#5578 = CLOSED_SHELL('',(#5530,#5531,#5532,#5533)) ;
#5579 = CLOSED_SHELL('',(#5534,#5535,#5536,#5537)) ;
#5580 = CLOSED_SHELL('',(#5538,#5539,#5540,#5541)) ;
#5581 = CLOSED_SHELL('',(#5542,#5543,#5544,#5545,#5546,#5547,#5548,#5549,
#5550,#5551)) ;
#5582 = CLOSED_SHELL('',(#5552,#5553,#5554,#5555,#5556,#5557,#5558,#5559,
#5560,#5561,#5562,#5563,#5564)) ;
#5583 = CLOSED_SHELL('',(#5565,#5566,#5567,#5568)) ;
#5584 = DERIVED_UNIT_ELEMENT(#5614,1.) ;
#5585 = DERIVED_UNIT_ELEMENT(#11398,-3.) ;
#5586 = DERIVED_UNIT_ELEMENT(#5614,1.) ;
#5587 = DERIVED_UNIT_ELEMENT(#11398,-3.) ;
#5588 = DERIVED_UNIT_ELEMENT(#5614,1.) ;
#5589 = DERIVED_UNIT_ELEMENT(#11398,-3.) ;
#5590 = DERIVED_UNIT_ELEMENT(#5614,1.) ;
#5591 = DERIVED_UNIT_ELEMENT(#11398,-3.) ;
#5592 = DERIVED_UNIT_ELEMENT(#5614,1.) ;
#5593 = DERIVED_UNIT_ELEMENT(#11398,-3.) ;
#5594 = DERIVED_UNIT_ELEMENT(#5614,1.) ;
#5595 = DERIVED_UNIT_ELEMENT(#11398,-3.) ;
#5596 = DERIVED_UNIT_ELEMENT(#5614,1.) ;
#5597 = DERIVED_UNIT_ELEMENT(#11398,-3.) ;
#5598 = DERIVED_UNIT_ELEMENT(#5614,1.) ;
#5599 = DERIVED_UNIT_ELEMENT(#11398,-3.) ;
#5600 = DERIVED_UNIT_ELEMENT(#5614,1.) ;
#5601 = DERIVED_UNIT_ELEMENT(#11398,-3.) ;
#5602 = DERIVED_UNIT_ELEMENT(#5614,1.) ;
#5603 = DERIVED_UNIT_ELEMENT(#11398,-3.) ;
#5604 = DERIVED_UNIT_ELEMENT(#5614,1.) ;
#5605 = DERIVED_UNIT_ELEMENT(#11398,-3.) ;
#5606 = DERIVED_UNIT_ELEMENT(#5614,1.) ;
#5607 = DERIVED_UNIT_ELEMENT(#11398,-3.) ;
#5608 = DERIVED_UNIT_ELEMENT(#5614,1.) ;
#5609 = DERIVED_UNIT_ELEMENT(#11398,-3.) ;
#5610 = DERIVED_UNIT_ELEMENT(#5614,1.) ;
#5611 = DERIVED_UNIT_ELEMENT(#11398,-3.) ;
#5612 = DERIVED_UNIT_ELEMENT(#5614,1.) ;
#5613 = DERIVED_UNIT_ELEMENT(#11398,-3.) ;
#5614 = (
MASS_UNIT()
NAMED_UNIT(*)
SI_UNIT(.KILO.,.GRAM.)
) ;
#5615 = DERIVED_UNIT((#5584,#5585)) ;
#5616 = DERIVED_UNIT((#5586,#5587)) ;
#5617 = DERIVED_UNIT((#5588,#5589)) ;
#5618 = DERIVED_UNIT((#5590,#5591)) ;
#5619 = DERIVED_UNIT((#5592,#5593)) ;
#5620 = DERIVED_UNIT((#5594,#5595)) ;
#5621 = DERIVED_UNIT((#5596,#5597)) ;
#5622 = DERIVED_UNIT((#5598,#5599)) ;
#5623 = DERIVED_UNIT((#5600,#5601)) ;
#5624 = DERIVED_UNIT((#5602,#5603)) ;
#5625 = DERIVED_UNIT((#5604,#5605)) ;
#5626 = DERIVED_UNIT((#5606,#5607)) ;
#5627 = DERIVED_UNIT((#5608,#5609)) ;
#5628 = DERIVED_UNIT((#5610,#5611)) ;
#5629 = DERIVED_UNIT((#5612,#5613)) ;
#5630 = MEASURE_REPRESENTATION_ITEM('density measure',
POSITIVE_RATIO_MEASURE(7850.),#5615) ;
#5631 = MEASURE_REPRESENTATION_ITEM('density measure',
POSITIVE_RATIO_MEASURE(7850.),#5616) ;
#5632 = MEASURE_REPRESENTATION_ITEM('density measure',
POSITIVE_RATIO_MEASURE(7850.),#5617) ;
#5633 = MEASURE_REPRESENTATION_ITEM('density measure',
POSITIVE_RATIO_MEASURE(7850.),#5618) ;
#5634 = MEASURE_REPRESENTATION_ITEM('density measure',
POSITIVE_RATIO_MEASURE(7850.),#5619) ;
#5635 = MEASURE_REPRESENTATION_ITEM('density measure',
POSITIVE_RATIO_MEASURE(7850.),#5620) ;
#5636 = MEASURE_REPRESENTATION_ITEM('density measure',
POSITIVE_RATIO_MEASURE(7850.),#5621) ;
#5637 = MEASURE_REPRESENTATION_ITEM('density measure',
POSITIVE_RATIO_MEASURE(7850.),#5622) ;
#5638 = MEASURE_REPRESENTATION_ITEM('density measure',
POSITIVE_RATIO_MEASURE(7850.),#5623) ;
#5639 = MEASURE_REPRESENTATION_ITEM('density measure',
POSITIVE_RATIO_MEASURE(7850.),#5624) ;
#5640 = MEASURE_REPRESENTATION_ITEM('density measure',
POSITIVE_RATIO_MEASURE(7850.),#5625) ;
#5641 = MEASURE_REPRESENTATION_ITEM('density measure',
POSITIVE_RATIO_MEASURE(7850.),#5626) ;
#5642 = MEASURE_REPRESENTATION_ITEM('density measure',
POSITIVE_RATIO_MEASURE(7850.),#5627) ;
#5643 = MEASURE_REPRESENTATION_ITEM('density measure',
POSITIVE_RATIO_MEASURE(7850.),#5628) ;
#5644 = MEASURE_REPRESENTATION_ITEM('density measure',
POSITIVE_RATIO_MEASURE(7850.),#5629) ;
#5645 = PROPERTY_DEFINITION_REPRESENTATION(#5720,#5675) ;
#5646 = PROPERTY_DEFINITION_REPRESENTATION(#5721,#5676) ;
#5647 = PROPERTY_DEFINITION_REPRESENTATION(#5722,#5677) ;
#5648 = PROPERTY_DEFINITION_REPRESENTATION(#5723,#5678) ;
#5649 = PROPERTY_DEFINITION_REPRESENTATION(#5724,#5679) ;
#5650 = PROPERTY_DEFINITION_REPRESENTATION(#5725,#5680) ;
#5651 = PROPERTY_DEFINITION_REPRESENTATION(#5726,#5681) ;
#5652 = PROPERTY_DEFINITION_REPRESENTATION(#5727,#5682) ;
#5653 = PROPERTY_DEFINITION_REPRESENTATION(#5728,#5683) ;
#5654 = PROPERTY_DEFINITION_REPRESENTATION(#5729,#5684) ;
#5655 = PROPERTY_DEFINITION_REPRESENTATION(#5730,#5685) ;
#5656 = PROPERTY_DEFINITION_REPRESENTATION(#5731,#5686) ;
#5657 = PROPERTY_DEFINITION_REPRESENTATION(#5732,#5687) ;
#5658 = PROPERTY_DEFINITION_REPRESENTATION(#5733,#5688) ;
#5659 = PROPERTY_DEFINITION_REPRESENTATION(#5734,#5689) ;
#5660 = PROPERTY_DEFINITION_REPRESENTATION(#5735,#5690) ;
#5661 = PROPERTY_DEFINITION_REPRESENTATION(#5736,#5691) ;
#5662 = PROPERTY_DEFINITION_REPRESENTATION(#5737,#5692) ;
#5663 = PROPERTY_DEFINITION_REPRESENTATION(#5738,#5693) ;
#5664 = PROPERTY_DEFINITION_REPRESENTATION(#5739,#5694) ;
#5665 = PROPERTY_DEFINITION_REPRESENTATION(#5740,#5695) ;
#5666 = PROPERTY_DEFINITION_REPRESENTATION(#5741,#5696) ;
#5667 = PROPERTY_DEFINITION_REPRESENTATION(#5742,#5697) ;
#5668 = PROPERTY_DEFINITION_REPRESENTATION(#5743,#5698) ;
#5669 = PROPERTY_DEFINITION_REPRESENTATION(#5744,#5699) ;
#5670 = PROPERTY_DEFINITION_REPRESENTATION(#5745,#5700) ;
#5671 = PROPERTY_DEFINITION_REPRESENTATION(#5746,#5701) ;
#5672 = PROPERTY_DEFINITION_REPRESENTATION(#5747,#5702) ;
#5673 = PROPERTY_DEFINITION_REPRESENTATION(#5748,#5703) ;
#5674 = PROPERTY_DEFINITION_REPRESENTATION(#5749,#5704) ;
#5675 = REPRESENTATION('material name',(#5705),#11381) ;
#5676 = REPRESENTATION('density',(#5630),#11381) ;
#5677 = REPRESENTATION('material name',(#5706),#11382) ;
#5678 = REPRESENTATION('density',(#5631),#11382) ;
#5679 = REPRESENTATION('material name',(#5707),#11383) ;
#5680 = REPRESENTATION('density',(#5632),#11383) ;
#5681 = REPRESENTATION('material name',(#5708),#11384) ;
#5682 = REPRESENTATION('density',(#5633),#11384) ;
#5683 = REPRESENTATION('material name',(#5709),#11385) ;
#5684 = REPRESENTATION('density',(#5634),#11385) ;
#5685 = REPRESENTATION('material name',(#5710),#11386) ;
#5686 = REPRESENTATION('density',(#5635),#11386) ;
#5687 = REPRESENTATION('material name',(#5711),#11387) ;
#5688 = REPRESENTATION('density',(#5636),#11387) ;
#5689 = REPRESENTATION('material name',(#5712),#11388) ;
#5690 = REPRESENTATION('density',(#5637),#11388) ;
#5691 = REPRESENTATION('material name',(#5713),#11389) ;
#5692 = REPRESENTATION('density',(#5638),#11389) ;
#5693 = REPRESENTATION('material name',(#5714),#11390) ;
#5694 = REPRESENTATION('density',(#5639),#11390) ;
#5695 = REPRESENTATION('material name',(#5715),#11391) ;
#5696 = REPRESENTATION('density',(#5640),#11391) ;
#5697 = REPRESENTATION('material name',(#5716),#11392) ;
#5698 = REPRESENTATION('density',(#5641),#11392) ;
#5699 = REPRESENTATION('material name',(#5717),#11393) ;
#5700 = REPRESENTATION('density',(#5642),#11393) ;
#5701 = REPRESENTATION('material name',(#5718),#11394) ;
#5702 = REPRESENTATION('density',(#5643),#11394) ;
#5703 = REPRESENTATION('material name',(#5719),#11395) ;
#5704 = REPRESENTATION('density',(#5644),#11395) ;
#5705 = DESCRIPTIVE_REPRESENTATION_ITEM('Steel','Steel') ;
#5706 = DESCRIPTIVE_REPRESENTATION_ITEM('Steel','Steel') ;
#5707 = DESCRIPTIVE_REPRESENTATION_ITEM('Steel','Steel') ;
#5708 = DESCRIPTIVE_REPRESENTATION_ITEM('Steel','Steel') ;
#5709 = DESCRIPTIVE_REPRESENTATION_ITEM('Steel','Steel') ;
#5710 = DESCRIPTIVE_REPRESENTATION_ITEM('Steel','Steel') ;
#5711 = DESCRIPTIVE_REPRESENTATION_ITEM('Steel','Steel') ;
#5712 = DESCRIPTIVE_REPRESENTATION_ITEM('Steel','Steel') ;
#5713 = DESCRIPTIVE_REPRESENTATION_ITEM('Steel','Steel') ;
#5714 = DESCRIPTIVE_REPRESENTATION_ITEM('Steel','Steel') ;
#5715 = DESCRIPTIVE_REPRESENTATION_ITEM('Steel','Steel') ;
#5716 = DESCRIPTIVE_REPRESENTATION_ITEM('Steel','Steel') ;
#5717 = DESCRIPTIVE_REPRESENTATION_ITEM('Steel','Steel') ;
#5718 = DESCRIPTIVE_REPRESENTATION_ITEM('Steel','Steel') ;
#5719 = DESCRIPTIVE_REPRESENTATION_ITEM('Steel','Steel') ;
#5720 = PROPERTY_DEFINITION('material property','material name',#11472) ;
#5721 = PROPERTY_DEFINITION('material property','density of part',#11472) ;
#5722 = PROPERTY_DEFINITION('material property','material name',#11473) ;
#5723 = PROPERTY_DEFINITION('material property','density of part',#11473) ;
#5724 = PROPERTY_DEFINITION('material property','material name',#11474) ;
#5725 = PROPERTY_DEFINITION('material property','density of part',#11474) ;
#5726 = PROPERTY_DEFINITION('material property','material name',#11475) ;
#5727 = PROPERTY_DEFINITION('material property','density of part',#11475) ;
#5728 = PROPERTY_DEFINITION('material property','material name',#11476) ;
#5729 = PROPERTY_DEFINITION('material property','density of part',#11476) ;
#5730 = PROPERTY_DEFINITION('material property','material name',#11477) ;
#5731 = PROPERTY_DEFINITION('material property','density of part',#11477) ;
#5732 = PROPERTY_DEFINITION('material property','material name',#11478) ;
#5733 = PROPERTY_DEFINITION('material property','density of part',#11478) ;
#5734 = PROPERTY_DEFINITION('material property','material name',#11479) ;
#5735 = PROPERTY_DEFINITION('material property','density of part',#11479) ;
#5736 = PROPERTY_DEFINITION('material property','material name',#11480) ;
#5737 = PROPERTY_DEFINITION('material property','density of part',#11480) ;
#5738 = PROPERTY_DEFINITION('material property','material name',#11481) ;
#5739 = PROPERTY_DEFINITION('material property','density of part',#11481) ;
#5740 = PROPERTY_DEFINITION('material property','material name',#11482) ;
#5741 = PROPERTY_DEFINITION('material property','density of part',#11482) ;
#5742 = PROPERTY_DEFINITION('material property','material name',#11483) ;
#5743 = PROPERTY_DEFINITION('material property','density of part',#11483) ;
#5744 = PROPERTY_DEFINITION('material property','material name',#11484) ;
#5745 = PROPERTY_DEFINITION('material property','density of part',#11484) ;
#5746 = PROPERTY_DEFINITION('material property','material name',#11485) ;
#5747 = PROPERTY_DEFINITION('material property','density of part',#11485) ;
#5748 = PROPERTY_DEFINITION('material property','material name',#11486) ;
#5749 = PROPERTY_DEFINITION('material property','density of part',#11486) ;
#5750 = AXIS2_PLACEMENT_3D('',#8128,#6415,#6416) ;
#5751 = AXIS2_PLACEMENT_3D('',#8129,#6417,#6418) ;
#5752 = AXIS2_PLACEMENT_3D('',#8130,#6419,#6420) ;
#5753 = AXIS2_PLACEMENT_3D('',#8132,#6421,#6422) ;
#5754 = AXIS2_PLACEMENT_3D('',#8135,#6424,#6425) ;
#5755 = AXIS2_PLACEMENT_3D('',#8136,#6426,#6427) ;
#5756 = AXIS2_PLACEMENT_3D('',#8138,#6428,#6429) ;
#5757 = AXIS2_PLACEMENT_3D('',#8141,#6431,#6432) ;
#5758 = AXIS2_PLACEMENT_3D('',#8142,#6433,#6434) ;
#5759 = AXIS2_PLACEMENT_3D('',#8144,#6435,#6436) ;
#5760 = AXIS2_PLACEMENT_3D('',#8147,#6438,#6439) ;
#5761 = AXIS2_PLACEMENT_3D('',#8148,#6440,#6441) ;
#5762 = AXIS2_PLACEMENT_3D('',#8151,#6442,#6443) ;
#5763 = AXIS2_PLACEMENT_3D('',#8159,#6447,#6448) ;
#5764 = AXIS2_PLACEMENT_3D('',#8161,#6450,#6451) ;
#5765 = AXIS2_PLACEMENT_3D('',#8175,#6459,#6460) ;
#5766 = AXIS2_PLACEMENT_3D('',#8179,#6463,#6464) ;
#5767 = AXIS2_PLACEMENT_3D('',#8183,#6467,#6468) ;
#5768 = AXIS2_PLACEMENT_3D('',#8187,#6471,#6472) ;
#5769 = AXIS2_PLACEMENT_3D('',#8191,#6475,#6476) ;
#5770 = AXIS2_PLACEMENT_3D('',#8197,#6480,#6481) ;
#5771 = AXIS2_PLACEMENT_3D('',#8203,#6485,#6486) ;
#5772 = AXIS2_PLACEMENT_3D('',#8205,#6487,#6488) ;
#5773 = AXIS2_PLACEMENT_3D('',#8207,#6489,#6490) ;
#5774 = AXIS2_PLACEMENT_3D('',#8210,#6492,#6493) ;
#5775 = AXIS2_PLACEMENT_3D('',#8211,#6494,#6495) ;
#5776 = AXIS2_PLACEMENT_3D('',#8234,#6497,#6498) ;
#5777 = AXIS2_PLACEMENT_3D('',#8237,#6499,#6500) ;
#5778 = AXIS2_PLACEMENT_3D('',#8239,#6501,#6502) ;
#5779 = AXIS2_PLACEMENT_3D('',#8241,#6503,#6504) ;
#5780 = AXIS2_PLACEMENT_3D('',#8242,#6505,#6506) ;
#5781 = AXIS2_PLACEMENT_3D('',#8243,#6507,#6508) ;
#5782 = AXIS2_PLACEMENT_3D('',#8246,#6509,#6510) ;
#5783 = AXIS2_PLACEMENT_3D('',#8249,#6513,#6514) ;
#5784 = AXIS2_PLACEMENT_3D('',#8252,#6515,#6516) ;
#5785 = AXIS2_PLACEMENT_3D('',#8253,#6517,#6518) ;
#5786 = AXIS2_PLACEMENT_3D('',#8254,#6519,#6520) ;
#5787 = AXIS2_PLACEMENT_3D('',#8255,#6521,#6522) ;
#5788 = AXIS2_PLACEMENT_3D('',#8258,#6525,#6526) ;
#5789 = AXIS2_PLACEMENT_3D('',#8264,#6530,#6531) ;
#5790 = AXIS2_PLACEMENT_3D('',#8267,#6533,#6534) ;
#5791 = AXIS2_PLACEMENT_3D('',#8268,#6535,#6536) ;
#5792 = AXIS2_PLACEMENT_3D('',#8271,#6537,#6538) ;
#5793 = AXIS2_PLACEMENT_3D('',#8275,#6540,#6541) ;
#5794 = AXIS2_PLACEMENT_3D('',#8282,#6545,#6546) ;
#5795 = AXIS2_PLACEMENT_3D('',#8283,#6547,#6548) ;
#5796 = AXIS2_PLACEMENT_3D('',#8285,#6549,#6550) ;
#5797 = AXIS2_PLACEMENT_3D('',#8287,#6551,#6552) ;
#5798 = AXIS2_PLACEMENT_3D('',#8288,#6553,#6554) ;
#5799 = AXIS2_PLACEMENT_3D('',#8289,#6555,#6556) ;
#5800 = AXIS2_PLACEMENT_3D('',#8292,#6558,#6559) ;
#5801 = AXIS2_PLACEMENT_3D('',#8293,#6560,#6561) ;
#5802 = AXIS2_PLACEMENT_3D('',#8295,#6562,#6563) ;
#5803 = AXIS2_PLACEMENT_3D('',#8297,#6564,#6565) ;
#5804 = AXIS2_PLACEMENT_3D('',#8299,#6566,#6567) ;
#5805 = AXIS2_PLACEMENT_3D('',#8300,#6568,#6569) ;
#5806 = AXIS2_PLACEMENT_3D('',#8301,#6570,#6571) ;
#5807 = AXIS2_PLACEMENT_3D('',#8308,#6574,#6575) ;
#5808 = AXIS2_PLACEMENT_3D('',#8312,#6577,#6578) ;
#5809 = AXIS2_PLACEMENT_3D('',#8316,#6580,#6581) ;
#5810 = AXIS2_PLACEMENT_3D('',#8320,#6583,#6584) ;
#5811 = AXIS2_PLACEMENT_3D('',#8322,#6586,#6587) ;
#5812 = AXIS2_PLACEMENT_3D('',#8325,#6589,#6590) ;
#5813 = AXIS2_PLACEMENT_3D('',#8326,#6591,#6592) ;
#5814 = AXIS2_PLACEMENT_3D('',#8328,#6593,#6594) ;
#5815 = AXIS2_PLACEMENT_3D('',#8330,#6595,#6596) ;
#5816 = AXIS2_PLACEMENT_3D('',#8331,#6597,#6598) ;
#5817 = AXIS2_PLACEMENT_3D('',#8332,#6599,#6600) ;
#5818 = AXIS2_PLACEMENT_3D('',#8334,#6601,#6602) ;
#5819 = AXIS2_PLACEMENT_3D('',#8336,#6604,#6605) ;
#5820 = AXIS2_PLACEMENT_3D('',#8338,#6606,#6607) ;
#5821 = AXIS2_PLACEMENT_3D('',#8339,#6608,#6609) ;
#5822 = AXIS2_PLACEMENT_3D('',#8340,#6610,#6611) ;
#5823 = AXIS2_PLACEMENT_3D('',#8342,#6613,#6614) ;
#5824 = AXIS2_PLACEMENT_3D('',#8348,#6618,#6619) ;
#5825 = AXIS2_PLACEMENT_3D('',#8351,#6621,#6622) ;
#5826 = AXIS2_PLACEMENT_3D('',#8378,#6623,#6624) ;
#5827 = AXIS2_PLACEMENT_3D('',#8379,#6625,#6626) ;
#5828 = AXIS2_PLACEMENT_3D('',#8380,#6627,#6628) ;
#5829 = AXIS2_PLACEMENT_3D('',#8383,#6629,#6630) ;
#5830 = AXIS2_PLACEMENT_3D('',#8386,#6633,#6634) ;
#5831 = AXIS2_PLACEMENT_3D('',#8388,#6635,#6636) ;
#5832 = AXIS2_PLACEMENT_3D('',#8391,#6638,#6639) ;
#5833 = AXIS2_PLACEMENT_3D('',#8392,#6640,#6641) ;
#5834 = AXIS2_PLACEMENT_3D('',#8393,#6642,#6643) ;
#5835 = AXIS2_PLACEMENT_3D('',#8394,#6644,#6645) ;
#5836 = AXIS2_PLACEMENT_3D('',#8395,#6646,#6647) ;
#5837 = AXIS2_PLACEMENT_3D('',#8398,#6648,#6649) ;
#5838 = AXIS2_PLACEMENT_3D('',#8439,#6650,#6651) ;
#5839 = AXIS2_PLACEMENT_3D('',#8482,#6652,#6653) ;
#5840 = AXIS2_PLACEMENT_3D('',#8483,#6654,#6655) ;
#5841 = AXIS2_PLACEMENT_3D('',#8524,#6657,#6658) ;
#5842 = AXIS2_PLACEMENT_3D('',#8593,#6659,#6660) ;
#5843 = AXIS2_PLACEMENT_3D('',#8630,#6661,#6662) ;
#5844 = AXIS2_PLACEMENT_3D('',#8633,#6663,#6664) ;
#5845 = AXIS2_PLACEMENT_3D('',#8634,#6665,#6666) ;
#5846 = AXIS2_PLACEMENT_3D('',#8635,#6667,#6668) ;
#5847 = AXIS2_PLACEMENT_3D('',#8664,#6669,#6670) ;
#5848 = AXIS2_PLACEMENT_3D('',#8666,#6671,#6672) ;
#5849 = AXIS2_PLACEMENT_3D('',#8667,#6673,#6674) ;
#5850 = AXIS2_PLACEMENT_3D('',#8701,#6675,#6676) ;
#5851 = AXIS2_PLACEMENT_3D('',#8703,#6677,#6678) ;
#5852 = AXIS2_PLACEMENT_3D('',#8716,#6679,#6680) ;
#5853 = AXIS2_PLACEMENT_3D('',#8718,#6682,#6683) ;
#5854 = AXIS2_PLACEMENT_3D('',#8721,#6685,#6686) ;
#5855 = AXIS2_PLACEMENT_3D('',#8722,#6687,#6688) ;
#5856 = AXIS2_PLACEMENT_3D('',#8724,#6689,#6690) ;
#5857 = AXIS2_PLACEMENT_3D('',#8726,#6692,#6693) ;
#5858 = AXIS2_PLACEMENT_3D('',#8728,#6694,#6695) ;
#5859 = AXIS2_PLACEMENT_3D('',#8731,#6697,#6698) ;
#5860 = AXIS2_PLACEMENT_3D('',#8732,#6699,#6700) ;
#5861 = AXIS2_PLACEMENT_3D('',#8735,#6701,#6702) ;
#5862 = AXIS2_PLACEMENT_3D('',#8736,#6703,#6704) ;
#5863 = AXIS2_PLACEMENT_3D('',#8737,#6705,#6706) ;
#5864 = AXIS2_PLACEMENT_3D('',#8738,#6707,#6708) ;
#5865 = AXIS2_PLACEMENT_3D('',#8741,#6709,#6710) ;
#5866 = AXIS2_PLACEMENT_3D('',#8791,#6713,#6714) ;
#5867 = AXIS2_PLACEMENT_3D('',#8792,#6715,#6716) ;
#5868 = AXIS2_PLACEMENT_3D('',#8793,#6717,#6718) ;
#5869 = AXIS2_PLACEMENT_3D('',#8794,#6719,#6720) ;
#5870 = AXIS2_PLACEMENT_3D('',#8795,#6721,#6722) ;
#5871 = AXIS2_PLACEMENT_3D('',#8796,#6723,#6724) ;
#5872 = AXIS2_PLACEMENT_3D('',#8797,#6725,#6726) ;
#5873 = AXIS2_PLACEMENT_3D('',#8805,#6730,#6731) ;
#5874 = AXIS2_PLACEMENT_3D('',#8807,#6733,#6734) ;
#5875 = AXIS2_PLACEMENT_3D('',#8808,#6735,#6736) ;
#5876 = AXIS2_PLACEMENT_3D('',#8809,#6737,#6738) ;
#5877 = AXIS2_PLACEMENT_3D('',#8811,#6740,#6741) ;
#5878 = AXIS2_PLACEMENT_3D('',#8813,#6742,#6743) ;
#5879 = AXIS2_PLACEMENT_3D('',#8815,#6745,#6746) ;
#5880 = AXIS2_PLACEMENT_3D('',#8817,#6748,#6749) ;
#5881 = AXIS2_PLACEMENT_3D('',#8823,#6752,#6753) ;
#5882 = AXIS2_PLACEMENT_3D('',#8827,#6756,#6757) ;
#5883 = AXIS2_PLACEMENT_3D('',#8828,#6758,#6759) ;
#5884 = AXIS2_PLACEMENT_3D('',#8829,#6760,#6761) ;
#5885 = AXIS2_PLACEMENT_3D('',#8830,#6762,#6763) ;
#5886 = AXIS2_PLACEMENT_3D('',#8833,#6764,#6765) ;
#5887 = AXIS2_PLACEMENT_3D('',#8901,#6766,#6767) ;
#5888 = AXIS2_PLACEMENT_3D('',#8903,#6769,#6770) ;
#5889 = AXIS2_PLACEMENT_3D('',#8905,#6771,#6772) ;
#5890 = AXIS2_PLACEMENT_3D('',#8930,#6774,#6775) ;
#5891 = AXIS2_PLACEMENT_3D('',#8932,#6777,#6778) ;
#5892 = AXIS2_PLACEMENT_3D('',#8936,#6781,#6782) ;
#5893 = AXIS2_PLACEMENT_3D('',#8939,#6784,#6785) ;
#5894 = AXIS2_PLACEMENT_3D('',#8940,#6786,#6787) ;
#5895 = AXIS2_PLACEMENT_3D('',#8944,#6790,#6791) ;
#5896 = AXIS2_PLACEMENT_3D('',#8969,#6793,#6794) ;
#5897 = AXIS2_PLACEMENT_3D('',#8970,#6795,#6796) ;
#5898 = AXIS2_PLACEMENT_3D('',#8989,#6797,#6798) ;
#5899 = AXIS2_PLACEMENT_3D('',#9039,#6799,#6800) ;
#5900 = AXIS2_PLACEMENT_3D('',#9040,#6801,#6802) ;
#5901 = AXIS2_PLACEMENT_3D('',#9041,#6803,#6804) ;
#5902 = AXIS2_PLACEMENT_3D('',#9045,#6807,#6808) ;
#5903 = AXIS2_PLACEMENT_3D('',#9046,#6809,#6810) ;
#5904 = AXIS2_PLACEMENT_3D('',#9047,#6811,#6812) ;
#5905 = AXIS2_PLACEMENT_3D('',#9051,#6815,#6816) ;
#5906 = AXIS2_PLACEMENT_3D('',#9052,#6817,#6818) ;
#5907 = AXIS2_PLACEMENT_3D('',#9053,#6819,#6820) ;
#5908 = AXIS2_PLACEMENT_3D('',#9059,#6824,#6825) ;
#5909 = AXIS2_PLACEMENT_3D('',#9062,#6827,#6828) ;
#5910 = AXIS2_PLACEMENT_3D('',#9063,#6829,#6830) ;
#5911 = AXIS2_PLACEMENT_3D('',#9067,#6833,#6834) ;
#5912 = AXIS2_PLACEMENT_3D('',#9070,#6836,#6837) ;
#5913 = AXIS2_PLACEMENT_3D('',#9071,#6838,#6839) ;
#5914 = AXIS2_PLACEMENT_3D('',#9075,#6842,#6843) ;
#5915 = AXIS2_PLACEMENT_3D('',#9078,#6845,#6846) ;
#5916 = AXIS2_PLACEMENT_3D('',#9079,#6847,#6848) ;
#5917 = AXIS2_PLACEMENT_3D('',#9083,#6851,#6852) ;
#5918 = AXIS2_PLACEMENT_3D('',#9086,#6854,#6855) ;
#5919 = AXIS2_PLACEMENT_3D('',#9087,#6856,#6857) ;
#5920 = AXIS2_PLACEMENT_3D('',#9091,#6860,#6861) ;
#5921 = AXIS2_PLACEMENT_3D('',#9092,#6862,#6863) ;
#5922 = AXIS2_PLACEMENT_3D('',#9093,#6864,#6865) ;
#5923 = AXIS2_PLACEMENT_3D('',#9094,#6866,#6867) ;
#5924 = AXIS2_PLACEMENT_3D('',#9095,#6868,#6869) ;
#5925 = AXIS2_PLACEMENT_3D('',#9111,#6871,#6872) ;
#5926 = AXIS2_PLACEMENT_3D('',#9114,#6874,#6875) ;
#5927 = AXIS2_PLACEMENT_3D('',#9115,#6876,#6877) ;
#5928 = AXIS2_PLACEMENT_3D('',#9124,#6878,#6879) ;
#5929 = AXIS2_PLACEMENT_3D('',#9125,#6880,#6881) ;
#5930 = AXIS2_PLACEMENT_3D('',#9126,#6882,#6883) ;
#5931 = AXIS2_PLACEMENT_3D('',#9128,#6884,#6885) ;
#5932 = AXIS2_PLACEMENT_3D('',#9132,#6887,#6888) ;
#5933 = AXIS2_PLACEMENT_3D('',#9135,#6890,#6891) ;
#5934 = AXIS2_PLACEMENT_3D('',#9136,#6892,#6893) ;
#5935 = AXIS2_PLACEMENT_3D('',#9139,#6894,#6895) ;
#5936 = AXIS2_PLACEMENT_3D('',#9141,#6896,#6897) ;
#5937 = AXIS2_PLACEMENT_3D('',#9149,#6898,#6899) ;
#5938 = AXIS2_PLACEMENT_3D('',#9150,#6900,#6901) ;
#5939 = AXIS2_PLACEMENT_3D('',#9153,#6902,#6903) ;
#5940 = AXIS2_PLACEMENT_3D('',#9167,#6906,#6907) ;
#5941 = AXIS2_PLACEMENT_3D('',#9171,#6909,#6910) ;
#5942 = AXIS2_PLACEMENT_3D('',#9174,#6912,#6913) ;
#5943 = AXIS2_PLACEMENT_3D('',#9176,#6914,#6915) ;
#5944 = AXIS2_PLACEMENT_3D('',#9177,#6916,#6917) ;
#5945 = AXIS2_PLACEMENT_3D('',#9180,#6918,#6919) ;
#5946 = AXIS2_PLACEMENT_3D('',#9182,#6920,#6921) ;
#5947 = AXIS2_PLACEMENT_3D('',#9184,#6922,#6923) ;
#5948 = AXIS2_PLACEMENT_3D('',#9185,#6924,#6925) ;
#5949 = AXIS2_PLACEMENT_3D('',#9186,#6926,#6927) ;
#5950 = AXIS2_PLACEMENT_3D('',#9189,#6928,#6929) ;
#5951 = AXIS2_PLACEMENT_3D('',#9192,#6932,#6933) ;
#5952 = AXIS2_PLACEMENT_3D('',#9195,#6934,#6935) ;
#5953 = AXIS2_PLACEMENT_3D('',#9196,#6936,#6937) ;
#5954 = AXIS2_PLACEMENT_3D('',#9197,#6938,#6939) ;
#5955 = AXIS2_PLACEMENT_3D('',#9198,#6940,#6941) ;
#5956 = AXIS2_PLACEMENT_3D('',#9201,#6944,#6945) ;
#5957 = AXIS2_PLACEMENT_3D('',#9207,#6949,#6950) ;
#5958 = AXIS2_PLACEMENT_3D('',#9210,#6952,#6953) ;
#5959 = AXIS2_PLACEMENT_3D('',#9211,#6954,#6955) ;
#5960 = AXIS2_PLACEMENT_3D('',#9215,#6957,#6958) ;
#5961 = AXIS2_PLACEMENT_3D('',#9219,#6960,#6961) ;
#5962 = AXIS2_PLACEMENT_3D('',#9221,#6962,#6963) ;
#5963 = AXIS2_PLACEMENT_3D('',#9223,#6964,#6965) ;
#5964 = AXIS2_PLACEMENT_3D('',#9227,#6967,#6968) ;
#5965 = AXIS2_PLACEMENT_3D('',#9232,#6971,#6972) ;
#5966 = AXIS2_PLACEMENT_3D('',#9236,#6974,#6975) ;
#5967 = AXIS2_PLACEMENT_3D('',#9238,#6977,#6978) ;
#5968 = AXIS2_PLACEMENT_3D('',#9240,#6979,#6980) ;
#5969 = AXIS2_PLACEMENT_3D('',#9242,#6981,#6982) ;
#5970 = AXIS2_PLACEMENT_3D('',#9243,#6983,#6984) ;
#5971 = AXIS2_PLACEMENT_3D('',#9244,#6985,#6986) ;
#5972 = AXIS2_PLACEMENT_3D('',#9246,#6987,#6988) ;
#5973 = AXIS2_PLACEMENT_3D('',#9248,#6990,#6991) ;
#5974 = AXIS2_PLACEMENT_3D('',#9250,#6992,#6993) ;
#5975 = AXIS2_PLACEMENT_3D('',#9251,#6994,#6995) ;
#5976 = AXIS2_PLACEMENT_3D('',#9252,#6996,#6997) ;
#5977 = AXIS2_PLACEMENT_3D('',#9254,#6999,#7000) ;
#5978 = AXIS2_PLACEMENT_3D('',#9260,#7004,#7005) ;
#5979 = AXIS2_PLACEMENT_3D('',#9263,#7007,#7008) ;
#5980 = AXIS2_PLACEMENT_3D('',#9264,#7009,#7010) ;
#5981 = AXIS2_PLACEMENT_3D('',#9266,#7012,#7013) ;
#5982 = AXIS2_PLACEMENT_3D('',#9268,#7015,#7016) ;
#5983 = AXIS2_PLACEMENT_3D('',#9271,#7017,#7018) ;
#5984 = AXIS2_PLACEMENT_3D('',#9312,#7019,#7020) ;
#5985 = AXIS2_PLACEMENT_3D('',#9315,#7022,#7023) ;
#5986 = AXIS2_PLACEMENT_3D('',#9316,#7024,#7025) ;
#5987 = AXIS2_PLACEMENT_3D('',#9318,#7026,#7027) ;
#5988 = AXIS2_PLACEMENT_3D('',#9319,#7028,#7029) ;
#5989 = AXIS2_PLACEMENT_3D('',#9320,#7030,#7031) ;
#5990 = AXIS2_PLACEMENT_3D('',#9322,#7033,#7034) ;
#5991 = AXIS2_PLACEMENT_3D('',#9325,#7035,#7036) ;
#5992 = AXIS2_PLACEMENT_3D('',#9326,#7037,#7038) ;
#5993 = AXIS2_PLACEMENT_3D('',#9339,#7039,#7040) ;
#5994 = AXIS2_PLACEMENT_3D('',#9340,#7041,#7042) ;
#5995 = AXIS2_PLACEMENT_3D('',#9341,#7043,#7044) ;
#5996 = AXIS2_PLACEMENT_3D('',#9344,#7046,#7047) ;
#5997 = AXIS2_PLACEMENT_3D('',#9345,#7048,#7049) ;
#5998 = AXIS2_PLACEMENT_3D('',#9347,#7050,#7051) ;
#5999 = AXIS2_PLACEMENT_3D('',#9348,#7052,#7053) ;
#6000 = AXIS2_PLACEMENT_3D('',#9349,#7054,#7055) ;
#6001 = AXIS2_PLACEMENT_3D('',#9351,#7057,#7058) ;
#6002 = AXIS2_PLACEMENT_3D('',#9359,#7063,#7064) ;
#6003 = AXIS2_PLACEMENT_3D('',#9362,#7066,#7067) ;
#6004 = AXIS2_PLACEMENT_3D('',#9363,#7068,#7069) ;
#6005 = AXIS2_PLACEMENT_3D('',#9367,#7072,#7073) ;
#6006 = AXIS2_PLACEMENT_3D('',#9370,#7075,#7076) ;
#6007 = AXIS2_PLACEMENT_3D('',#9371,#7077,#7078) ;
#6008 = AXIS2_PLACEMENT_3D('',#9374,#7080,#7081) ;
#6009 = AXIS2_PLACEMENT_3D('',#9375,#7082,#7083) ;
#6010 = AXIS2_PLACEMENT_3D('',#9378,#7085,#7086) ;
#6011 = AXIS2_PLACEMENT_3D('',#9379,#7087,#7088) ;
#6012 = AXIS2_PLACEMENT_3D('',#9383,#7091,#7092) ;
#6013 = AXIS2_PLACEMENT_3D('',#9386,#7094,#7095) ;
#6014 = AXIS2_PLACEMENT_3D('',#9387,#7096,#7097) ;
#6015 = AXIS2_PLACEMENT_3D('',#9393,#7101,#7102) ;
#6016 = AXIS2_PLACEMENT_3D('',#9396,#7104,#7105) ;
#6017 = AXIS2_PLACEMENT_3D('',#9397,#7106,#7107) ;
#6018 = AXIS2_PLACEMENT_3D('',#9399,#7108,#7109) ;
#6019 = AXIS2_PLACEMENT_3D('',#9401,#7111,#7112) ;
#6020 = AXIS2_PLACEMENT_3D('',#9409,#7116,#7117) ;
#6021 = AXIS2_PLACEMENT_3D('',#9412,#7119,#7120) ;
#6022 = AXIS2_PLACEMENT_3D('',#9413,#7121,#7122) ;
#6023 = AXIS2_PLACEMENT_3D('',#9419,#7126,#7127) ;
#6024 = AXIS2_PLACEMENT_3D('',#9423,#7130,#7131) ;
#6025 = AXIS2_PLACEMENT_3D('',#9425,#7132,#7133) ;
#6026 = AXIS2_PLACEMENT_3D('',#9427,#7135,#7136) ;
#6027 = AXIS2_PLACEMENT_3D('',#9431,#7139,#7140) ;
#6028 = AXIS2_PLACEMENT_3D('',#9432,#7141,#7142) ;
#6029 = AXIS2_PLACEMENT_3D('',#9434,#7144,#7145) ;
#6030 = AXIS2_PLACEMENT_3D('',#9437,#7147,#7148) ;
#6031 = AXIS2_PLACEMENT_3D('',#9440,#7150,#7151) ;
#6032 = AXIS2_PLACEMENT_3D('',#9441,#7152,#7153) ;
#6033 = AXIS2_PLACEMENT_3D('',#9443,#7155,#7156) ;
#6034 = AXIS2_PLACEMENT_3D('',#9444,#7157,#7158) ;
#6035 = AXIS2_PLACEMENT_3D('',#9446,#7160,#7161) ;
#6036 = AXIS2_PLACEMENT_3D('',#9447,#7162,#7163) ;
#6037 = AXIS2_PLACEMENT_3D('',#9449,#7165,#7166) ;
#6038 = AXIS2_PLACEMENT_3D('',#9450,#7167,#7168) ;
#6039 = AXIS2_PLACEMENT_3D('',#9451,#7169,#7170) ;
#6040 = AXIS2_PLACEMENT_3D('',#9492,#7173,#7174) ;
#6041 = AXIS2_PLACEMENT_3D('',#9506,#7175,#7176) ;
#6042 = AXIS2_PLACEMENT_3D('',#9507,#7177,#7178) ;
#6043 = AXIS2_PLACEMENT_3D('',#9524,#7181,#7182) ;
#6044 = AXIS2_PLACEMENT_3D('',#9526,#7183,#7184) ;
#6045 = AXIS2_PLACEMENT_3D('',#9540,#7185,#7186) ;
#6046 = AXIS2_PLACEMENT_3D('',#9541,#7187,#7188) ;
#6047 = AXIS2_PLACEMENT_3D('',#9558,#7191,#7192) ;
#6048 = AXIS2_PLACEMENT_3D('',#9587,#7193,#7194) ;
#6049 = AXIS2_PLACEMENT_3D('',#9601,#7195,#7196) ;
#6050 = AXIS2_PLACEMENT_3D('',#9602,#7197,#7198) ;
#6051 = AXIS2_PLACEMENT_3D('',#9619,#7201,#7202) ;
#6052 = AXIS2_PLACEMENT_3D('',#9621,#7203,#7204) ;
#6053 = AXIS2_PLACEMENT_3D('',#9635,#7205,#7206) ;
#6054 = AXIS2_PLACEMENT_3D('',#9636,#7207,#7208) ;
#6055 = AXIS2_PLACEMENT_3D('',#9666,#7211,#7212) ;
#6056 = AXIS2_PLACEMENT_3D('',#9668,#7213,#7214) ;
#6057 = AXIS2_PLACEMENT_3D('',#9682,#7215,#7216) ;
#6058 = AXIS2_PLACEMENT_3D('',#9683,#7217,#7218) ;
#6059 = AXIS2_PLACEMENT_3D('',#9731,#7221,#7222) ;
#6060 = AXIS2_PLACEMENT_3D('',#9763,#7225,#7226) ;
#6061 = AXIS2_PLACEMENT_3D('',#9764,#7227,#7228) ;
#6062 = AXIS2_PLACEMENT_3D('',#9766,#7229,#7230) ;
#6063 = AXIS2_PLACEMENT_3D('',#9780,#7231,#7232) ;
#6064 = AXIS2_PLACEMENT_3D('',#9781,#7233,#7234) ;
#6065 = AXIS2_PLACEMENT_3D('',#9783,#7235,#7236) ;
#6066 = AXIS2_PLACEMENT_3D('',#9810,#7237,#7238) ;
#6067 = AXIS2_PLACEMENT_3D('',#9811,#7239,#7240) ;
#6068 = AXIS2_PLACEMENT_3D('',#9813,#7241,#7242) ;
#6069 = AXIS2_PLACEMENT_3D('',#9827,#7243,#7244) ;
#6070 = AXIS2_PLACEMENT_3D('',#9828,#7245,#7246) ;
#6071 = AXIS2_PLACEMENT_3D('',#9857,#7247,#7248) ;
#6072 = AXIS2_PLACEMENT_3D('',#9859,#7249,#7250) ;
#6073 = AXIS2_PLACEMENT_3D('',#9860,#7251,#7252) ;
#6074 = AXIS2_PLACEMENT_3D('',#9861,#7253,#7254) ;
#6075 = AXIS2_PLACEMENT_3D('',#9864,#7257,#7258) ;
#6076 = AXIS2_PLACEMENT_3D('',#9867,#7261,#7262) ;
#6077 = AXIS2_PLACEMENT_3D('',#9884,#7265,#7266) ;
#6078 = AXIS2_PLACEMENT_3D('',#9912,#7267,#7268) ;
#6079 = AXIS2_PLACEMENT_3D('',#9913,#7269,#7270) ;
#6080 = AXIS2_PLACEMENT_3D('',#9914,#7271,#7272) ;
#6081 = AXIS2_PLACEMENT_3D('',#9916,#7273,#7274) ;
#6082 = AXIS2_PLACEMENT_3D('',#9918,#7275,#7276) ;
#6083 = AXIS2_PLACEMENT_3D('',#9933,#7277,#7278) ;
#6084 = AXIS2_PLACEMENT_3D('',#9936,#7281,#7282) ;
#6085 = AXIS2_PLACEMENT_3D('',#9938,#7283,#7284) ;
#6086 = AXIS2_PLACEMENT_3D('',#9940,#7285,#7286) ;
#6087 = AXIS2_PLACEMENT_3D('',#9941,#7287,#7288) ;
#6088 = AXIS2_PLACEMENT_3D('',#9942,#7289,#7290) ;
#6089 = AXIS2_PLACEMENT_3D('',#9945,#7293,#7294) ;
#6090 = AXIS2_PLACEMENT_3D('',#9947,#7295,#7296) ;
#6091 = AXIS2_PLACEMENT_3D('',#9949,#7297,#7298) ;
#6092 = AXIS2_PLACEMENT_3D('',#9964,#7299,#7300) ;
#6093 = AXIS2_PLACEMENT_3D('',#9983,#7303,#7304) ;
#6094 = AXIS2_PLACEMENT_3D('',#9985,#7305,#7306) ;
#6095 = AXIS2_PLACEMENT_3D('',#10001,#7307,#7308) ;
#6096 = AXIS2_PLACEMENT_3D('',#10002,#7309,#7310) ;
#6097 = AXIS2_PLACEMENT_3D('',#10019,#7313,#7314) ;
#6098 = AXIS2_PLACEMENT_3D('',#10020,#7315,#7316) ;
#6099 = AXIS2_PLACEMENT_3D('',#10021,#7317,#7318) ;
#6100 = AXIS2_PLACEMENT_3D('',#10022,#7319,#7320) ;
#6101 = AXIS2_PLACEMENT_3D('',#10026,#7322,#7323) ;
#6102 = AXIS2_PLACEMENT_3D('',#10028,#7325,#7326) ;
#6103 = AXIS2_PLACEMENT_3D('',#10032,#7329,#7330) ;
#6104 = AXIS2_PLACEMENT_3D('',#10035,#7332,#7333) ;
#6105 = AXIS2_PLACEMENT_3D('',#10036,#7334,#7335) ;
#6106 = AXIS2_PLACEMENT_3D('',#10040,#7338,#7339) ;
#6107 = AXIS2_PLACEMENT_3D('',#10043,#7341,#7342) ;
#6108 = AXIS2_PLACEMENT_3D('',#10044,#7343,#7344) ;
#6109 = AXIS2_PLACEMENT_3D('',#10048,#7347,#7348) ;
#6110 = AXIS2_PLACEMENT_3D('',#10051,#7350,#7351) ;
#6111 = AXIS2_PLACEMENT_3D('',#10052,#7352,#7353) ;
#6112 = AXIS2_PLACEMENT_3D('',#10055,#7355,#7356) ;
#6113 = AXIS2_PLACEMENT_3D('',#10056,#7357,#7358) ;
#6114 = AXIS2_PLACEMENT_3D('',#10060,#7361,#7362) ;
#6115 = AXIS2_PLACEMENT_3D('',#10063,#7364,#7365) ;
#6116 = AXIS2_PLACEMENT_3D('',#10064,#7366,#7367) ;
#6117 = AXIS2_PLACEMENT_3D('',#10068,#7370,#7371) ;
#6118 = AXIS2_PLACEMENT_3D('',#10071,#7373,#7374) ;
#6119 = AXIS2_PLACEMENT_3D('',#10072,#7375,#7376) ;
#6120 = AXIS2_PLACEMENT_3D('',#10075,#7378,#7379) ;
#6121 = AXIS2_PLACEMENT_3D('',#10076,#7380,#7381) ;
#6122 = AXIS2_PLACEMENT_3D('',#10080,#7384,#7385) ;
#6123 = AXIS2_PLACEMENT_3D('',#10083,#7387,#7388) ;
#6124 = AXIS2_PLACEMENT_3D('',#10084,#7389,#7390) ;
#6125 = AXIS2_PLACEMENT_3D('',#10089,#7392,#7393) ;
#6126 = AXIS2_PLACEMENT_3D('',#10092,#7395,#7396) ;
#6127 = AXIS2_PLACEMENT_3D('',#10094,#7397,#7398) ;
#6128 = AXIS2_PLACEMENT_3D('',#10095,#7399,#7400) ;
#6129 = AXIS2_PLACEMENT_3D('',#10098,#7401,#7402) ;
#6130 = AXIS2_PLACEMENT_3D('',#10123,#7403,#7404) ;
#6131 = AXIS2_PLACEMENT_3D('',#10142,#7407,#7408) ;
#6132 = AXIS2_PLACEMENT_3D('',#10144,#7409,#7410) ;
#6133 = AXIS2_PLACEMENT_3D('',#10158,#7411,#7412) ;
#6134 = AXIS2_PLACEMENT_3D('',#10159,#7413,#7414) ;
#6135 = AXIS2_PLACEMENT_3D('',#10176,#7417,#7418) ;
#6136 = AXIS2_PLACEMENT_3D('',#10178,#7419,#7420) ;
#6137 = AXIS2_PLACEMENT_3D('',#10192,#7421,#7422) ;
#6138 = AXIS2_PLACEMENT_3D('',#10193,#7423,#7424) ;
#6139 = AXIS2_PLACEMENT_3D('',#10234,#7426,#7427) ;
#6140 = AXIS2_PLACEMENT_3D('',#10263,#7428,#7429) ;
#6141 = AXIS2_PLACEMENT_3D('',#10265,#7430,#7431) ;
#6142 = AXIS2_PLACEMENT_3D('',#10266,#7432,#7433) ;
#6143 = AXIS2_PLACEMENT_3D('',#10267,#7434,#7435) ;
#6144 = AXIS2_PLACEMENT_3D('',#10286,#7438,#7439) ;
#6145 = AXIS2_PLACEMENT_3D('',#10313,#7440,#7441) ;
#6146 = AXIS2_PLACEMENT_3D('',#10314,#7442,#7443) ;
#6147 = AXIS2_PLACEMENT_3D('',#10316,#7444,#7445) ;
#6148 = AXIS2_PLACEMENT_3D('',#10330,#7446,#7447) ;
#6149 = AXIS2_PLACEMENT_3D('',#10331,#7448,#7449) ;
#6150 = AXIS2_PLACEMENT_3D('',#10335,#7451,#7452) ;
#6151 = AXIS2_PLACEMENT_3D('',#10337,#7454,#7455) ;
#6152 = AXIS2_PLACEMENT_3D('',#10365,#7456,#7457) ;
#6153 = AXIS2_PLACEMENT_3D('',#10366,#7458,#7459) ;
#6154 = AXIS2_PLACEMENT_3D('',#10367,#7460,#7461) ;
#6155 = AXIS2_PLACEMENT_3D('',#10397,#7464,#7465) ;
#6156 = AXIS2_PLACEMENT_3D('',#10412,#7467,#7468) ;
#6157 = AXIS2_PLACEMENT_3D('',#10440,#7469,#7470) ;
#6158 = AXIS2_PLACEMENT_3D('',#10441,#7471,#7472) ;
#6159 = AXIS2_PLACEMENT_3D('',#10442,#7473,#7474) ;
#6160 = AXIS2_PLACEMENT_3D('',#10444,#7475,#7476) ;
#6161 = AXIS2_PLACEMENT_3D('',#10457,#7477,#7478) ;
#6162 = AXIS2_PLACEMENT_3D('',#10460,#7481,#7482) ;
#6163 = AXIS2_PLACEMENT_3D('',#10462,#7483,#7484) ;
#6164 = AXIS2_PLACEMENT_3D('',#10475,#7485,#7486) ;
#6165 = AXIS2_PLACEMENT_3D('',#10477,#7488,#7489) ;
#6166 = AXIS2_PLACEMENT_3D('',#10507,#7492,#7493) ;
#6167 = AXIS2_PLACEMENT_3D('',#10509,#7494,#7495) ;
#6168 = AXIS2_PLACEMENT_3D('',#10522,#7496,#7497) ;
#6169 = AXIS2_PLACEMENT_3D('',#10539,#7500,#7501) ;
#6170 = AXIS2_PLACEMENT_3D('',#10540,#7502,#7503) ;
#6171 = AXIS2_PLACEMENT_3D('',#10541,#7504,#7505) ;
#6172 = AXIS2_PLACEMENT_3D('',#10542,#7506,#7507) ;
#6173 = AXIS2_PLACEMENT_3D('',#10544,#7508,#7509) ;
#6174 = AXIS2_PLACEMENT_3D('',#10557,#7510,#7511) ;
#6175 = AXIS2_PLACEMENT_3D('',#10572,#7513,#7514) ;
#6176 = AXIS2_PLACEMENT_3D('',#10574,#7515,#7516) ;
#6177 = AXIS2_PLACEMENT_3D('',#10587,#7517,#7518) ;
#6178 = AXIS2_PLACEMENT_3D('',#10612,#7520,#7521) ;
#6179 = AXIS2_PLACEMENT_3D('',#10625,#7522,#7523) ;
#6180 = AXIS2_PLACEMENT_3D('',#10627,#7525,#7526) ;
#6181 = AXIS2_PLACEMENT_3D('',#10629,#7528,#7529) ;
#6182 = AXIS2_PLACEMENT_3D('',#10631,#7531,#7532) ;
#6183 = AXIS2_PLACEMENT_3D('',#10633,#7534,#7535) ;
#6184 = AXIS2_PLACEMENT_3D('',#10635,#7537,#7538) ;
#6185 = AXIS2_PLACEMENT_3D('',#10637,#7540,#7541) ;
#6186 = AXIS2_PLACEMENT_3D('',#10639,#7543,#7544) ;
#6187 = AXIS2_PLACEMENT_3D('',#10641,#7546,#7547) ;
#6188 = AXIS2_PLACEMENT_3D('',#10643,#7549,#7550) ;
#6189 = AXIS2_PLACEMENT_3D('',#10645,#7552,#7553) ;
#6190 = AXIS2_PLACEMENT_3D('',#10647,#7555,#7556) ;
#6191 = AXIS2_PLACEMENT_3D('',#10649,#7558,#7559) ;
#6192 = AXIS2_PLACEMENT_3D('',#10651,#7561,#7562) ;
#6193 = AXIS2_PLACEMENT_3D('',#10653,#7564,#7565) ;
#6194 = AXIS2_PLACEMENT_3D('',#10654,#7566,#7567) ;
#6195 = AXIS2_PLACEMENT_3D('',#10657,#7568,#7569) ;
#6196 = AXIS2_PLACEMENT_3D('',#10661,#7571,#7572) ;
#6197 = AXIS2_PLACEMENT_3D('',#10664,#7574,#7575) ;
#6198 = AXIS2_PLACEMENT_3D('',#10665,#7576,#7577) ;
#6199 = AXIS2_PLACEMENT_3D('',#10693,#7579,#7580) ;
#6200 = AXIS2_PLACEMENT_3D('',#10707,#7581,#7582) ;
#6201 = AXIS2_PLACEMENT_3D('',#10708,#7583,#7584) ;
#6202 = AXIS2_PLACEMENT_3D('',#10723,#7586,#7587) ;
#6203 = AXIS2_PLACEMENT_3D('',#10724,#7588,#7589) ;
#6204 = AXIS2_PLACEMENT_3D('',#10725,#7590,#7591) ;
#6205 = AXIS2_PLACEMENT_3D('',#10729,#7593,#7594) ;
#6206 = AXIS2_PLACEMENT_3D('',#10731,#7596,#7597) ;
#6207 = AXIS2_PLACEMENT_3D('',#10735,#7600,#7601) ;
#6208 = AXIS2_PLACEMENT_3D('',#10737,#7602,#7603) ;
#6209 = AXIS2_PLACEMENT_3D('',#10762,#7604,#7605) ;
#6210 = AXIS2_PLACEMENT_3D('',#10787,#7606,#7607) ;
#6211 = AXIS2_PLACEMENT_3D('',#10789,#7609,#7610) ;
#6212 = AXIS2_PLACEMENT_3D('',#10790,#7611,#7612) ;
#6213 = AXIS2_PLACEMENT_3D('',#10792,#7614,#7615) ;
#6214 = AXIS2_PLACEMENT_3D('',#10794,#7617,#7618) ;
#6215 = AXIS2_PLACEMENT_3D('',#10795,#7619,#7620) ;
#6216 = AXIS2_PLACEMENT_3D('',#10796,#7621,#7622) ;
#6217 = AXIS2_PLACEMENT_3D('',#10798,#7623,#7624) ;
#6218 = AXIS2_PLACEMENT_3D('',#10799,#7625,#7626) ;
#6219 = AXIS2_PLACEMENT_3D('',#10801,#7627,#7628) ;
#6220 = AXIS2_PLACEMENT_3D('',#10803,#7630,#7631) ;
#6221 = AXIS2_PLACEMENT_3D('',#10805,#7632,#7633) ;
#6222 = AXIS2_PLACEMENT_3D('',#10807,#7635,#7636) ;
#6223 = AXIS2_PLACEMENT_3D('',#10809,#7637,#7638) ;
#6224 = AXIS2_PLACEMENT_3D('',#10811,#7640,#7641) ;
#6225 = AXIS2_PLACEMENT_3D('',#10812,#7642,#7643) ;
#6226 = AXIS2_PLACEMENT_3D('',#10813,#7644,#7645) ;
#6227 = AXIS2_PLACEMENT_3D('',#10815,#7646,#7647) ;
#6228 = AXIS2_PLACEMENT_3D('',#10816,#7648,#7649) ;
#6229 = AXIS2_PLACEMENT_3D('',#10818,#7650,#7651) ;
#6230 = AXIS2_PLACEMENT_3D('',#10820,#7653,#7654) ;
#6231 = AXIS2_PLACEMENT_3D('',#10822,#7655,#7656) ;
#6232 = AXIS2_PLACEMENT_3D('',#10823,#7657,#7658) ;
#6233 = AXIS2_PLACEMENT_3D('',#10825,#7659,#7660) ;
#6234 = AXIS2_PLACEMENT_3D('',#10827,#7662,#7663) ;
#6235 = AXIS2_PLACEMENT_3D('',#10829,#7664,#7665) ;
#6236 = AXIS2_PLACEMENT_3D('',#10831,#7667,#7668) ;
#6237 = AXIS2_PLACEMENT_3D('',#10833,#7669,#7670) ;
#6238 = AXIS2_PLACEMENT_3D('',#10835,#7672,#7673) ;
#6239 = AXIS2_PLACEMENT_3D('',#10837,#7674,#7675) ;
#6240 = AXIS2_PLACEMENT_3D('',#10838,#7676,#7677) ;
#6241 = AXIS2_PLACEMENT_3D('',#10840,#7678,#7679) ;
#6242 = AXIS2_PLACEMENT_3D('',#10842,#7681,#7682) ;
#6243 = AXIS2_PLACEMENT_3D('',#10843,#7683,#7684) ;
#6244 = AXIS2_PLACEMENT_3D('',#10844,#7685,#7686) ;
#6245 = AXIS2_PLACEMENT_3D('',#10846,#7687,#7688) ;
#6246 = AXIS2_PLACEMENT_3D('',#10847,#7689,#7690) ;
#6247 = AXIS2_PLACEMENT_3D('',#10849,#7691,#7692) ;
#6248 = AXIS2_PLACEMENT_3D('',#10851,#7694,#7695) ;
#6249 = AXIS2_PLACEMENT_3D('',#10853,#7696,#7697) ;
#6250 = AXIS2_PLACEMENT_3D('',#10855,#7699,#7700) ;
#6251 = AXIS2_PLACEMENT_3D('',#10857,#7701,#7702) ;
#6252 = AXIS2_PLACEMENT_3D('',#10859,#7704,#7705) ;
#6253 = AXIS2_PLACEMENT_3D('',#10860,#7706,#7707) ;
#6254 = AXIS2_PLACEMENT_3D('',#10861,#7708,#7709) ;
#6255 = AXIS2_PLACEMENT_3D('',#10863,#7710,#7711) ;
#6256 = AXIS2_PLACEMENT_3D('',#10866,#7713,#7714) ;
#6257 = AXIS2_PLACEMENT_3D('',#10867,#7715,#7716) ;
#6258 = AXIS2_PLACEMENT_3D('',#10876,#7721,#7722) ;
#6259 = AXIS2_PLACEMENT_3D('',#10882,#7726,#7727) ;
#6260 = AXIS2_PLACEMENT_3D('',#10888,#7731,#7732) ;
#6261 = AXIS2_PLACEMENT_3D('',#10894,#7736,#7737) ;
#6262 = AXIS2_PLACEMENT_3D('',#10900,#7741,#7742) ;
#6263 = AXIS2_PLACEMENT_3D('',#10906,#7746,#7747) ;
#6264 = AXIS2_PLACEMENT_3D('',#10912,#7751,#7752) ;
#6265 = AXIS2_PLACEMENT_3D('',#10918,#7756,#7757) ;
#6266 = AXIS2_PLACEMENT_3D('',#10921,#7760,#7761) ;
#6267 = AXIS2_PLACEMENT_3D('',#10922,#7762,#7763) ;
#6268 = AXIS2_PLACEMENT_3D('',#10923,#7764,#7765) ;
#6269 = AXIS2_PLACEMENT_3D('',#10924,#7766,#7767) ;
#6270 = AXIS2_PLACEMENT_3D('',#10933,#7772,#7773) ;
#6271 = AXIS2_PLACEMENT_3D('',#10939,#7777,#7778) ;
#6272 = AXIS2_PLACEMENT_3D('',#10945,#7782,#7783) ;
#6273 = AXIS2_PLACEMENT_3D('',#10951,#7787,#7788) ;
#6274 = AXIS2_PLACEMENT_3D('',#10957,#7792,#7793) ;
#6275 = AXIS2_PLACEMENT_3D('',#10960,#7796,#7797) ;
#6276 = AXIS2_PLACEMENT_3D('',#10961,#7798,#7799) ;
#6277 = AXIS2_PLACEMENT_3D('',#10963,#7800,#7801) ;
#6278 = AXIS2_PLACEMENT_3D('',#10964,#7802,#7803) ;
#6279 = AXIS2_PLACEMENT_3D('',#10966,#7804,#7805) ;
#6280 = AXIS2_PLACEMENT_3D('',#10968,#7807,#7808) ;
#6281 = AXIS2_PLACEMENT_3D('',#10970,#7809,#7810) ;
#6282 = AXIS2_PLACEMENT_3D('',#10972,#7812,#7813) ;
#6283 = AXIS2_PLACEMENT_3D('',#10974,#7814,#7815) ;
#6284 = AXIS2_PLACEMENT_3D('',#10976,#7817,#7818) ;
#6285 = AXIS2_PLACEMENT_3D('',#10978,#7819,#7820) ;
#6286 = AXIS2_PLACEMENT_3D('',#10980,#7822,#7823) ;
#6287 = AXIS2_PLACEMENT_3D('',#10982,#7824,#7825) ;
#6288 = AXIS2_PLACEMENT_3D('',#10984,#7827,#7828) ;
#6289 = AXIS2_PLACEMENT_3D('',#10985,#7829,#7830) ;
#6290 = AXIS2_PLACEMENT_3D('',#10986,#7831,#7832) ;
#6291 = AXIS2_PLACEMENT_3D('',#10988,#7833,#7834) ;
#6292 = AXIS2_PLACEMENT_3D('',#11076,#7836,#7837) ;
#6293 = AXIS2_PLACEMENT_3D('',#11079,#7839,#7840) ;
#6294 = AXIS2_PLACEMENT_3D('',#11081,#7841,#7842) ;
#6295 = AXIS2_PLACEMENT_3D('',#11083,#7843,#7844) ;
#6296 = AXIS2_PLACEMENT_3D('',#11084,#7845,#7846) ;
#6297 = AXIS2_PLACEMENT_3D('',#11085,#7847,#7848) ;
#6298 = AXIS2_PLACEMENT_3D('',#11086,#7849,#7850) ;
#6299 = AXIS2_PLACEMENT_3D('',#11088,#7851,#7852) ;
#6300 = AXIS2_PLACEMENT_3D('',#11090,#7853,#7854) ;
#6301 = AXIS2_PLACEMENT_3D('',#11120,#7855,#7856) ;
#6302 = AXIS2_PLACEMENT_3D('',#11121,#7857,#7858) ;
#6303 = AXIS2_PLACEMENT_3D('',#11123,#7859,#7860) ;
#6304 = AXIS2_PLACEMENT_3D('',#11152,#7862,#7863) ;
#6305 = AXIS2_PLACEMENT_3D('',#11153,#7864,#7865) ;
#6306 = AXIS2_PLACEMENT_3D('',#11156,#7867,#7868) ;
#6307 = AXIS2_PLACEMENT_3D('',#11158,#7869,#7870) ;
#6308 = AXIS2_PLACEMENT_3D('',#11159,#7871,#7872) ;
#6309 = AXIS2_PLACEMENT_3D('',#11160,#7873,#7874) ;
#6310 = AXIS2_PLACEMENT_3D('',#11161,#7875,#7876) ;
#6311 = AXIS2_PLACEMENT_3D('',#11162,#7877,#7878) ;
#6312 = AXIS2_PLACEMENT_3D('',#11163,#7879,#7880) ;
#6313 = AXIS2_PLACEMENT_3D('',#11165,#7881,#7882) ;
#6314 = AXIS2_PLACEMENT_3D('',#11168,#7884,#7885) ;
#6315 = AXIS2_PLACEMENT_3D('',#11169,#7886,#7887) ;
#6316 = AXIS2_PLACEMENT_3D('',#11171,#7888,#7889) ;
#6317 = AXIS2_PLACEMENT_3D('',#11172,#7890,#7891) ;
#6318 = AXIS2_PLACEMENT_3D('',#11174,#7892,#7893) ;
#6319 = AXIS2_PLACEMENT_3D('',#11176,#7895,#7896) ;
#6320 = AXIS2_PLACEMENT_3D('',#11177,#7897,#7898) ;
#6321 = AXIS2_PLACEMENT_3D('',#11178,#7899,#7900) ;
#6322 = AXIS2_PLACEMENT_3D('',#11180,#7901,#7902) ;
#6323 = AXIS2_PLACEMENT_3D('',#11183,#7904,#7905) ;
#6324 = AXIS2_PLACEMENT_3D('',#11184,#7906,#7907) ;
#6325 = AXIS2_PLACEMENT_3D('',#11186,#7908,#7909) ;
#6326 = AXIS2_PLACEMENT_3D('',#11187,#7910,#7911) ;
#6327 = AXIS2_PLACEMENT_3D('',#11189,#7912,#7913) ;
#6328 = AXIS2_PLACEMENT_3D('',#11191,#7915,#7916) ;
#6329 = AXIS2_PLACEMENT_3D('',#11192,#7917,#7918) ;
#6330 = AXIS2_PLACEMENT_3D('',#11193,#7919,#7920) ;
#6331 = AXIS2_PLACEMENT_3D('',#11195,#7921,#7922) ;
#6332 = AXIS2_PLACEMENT_3D('',#11198,#7924,#7925) ;
#6333 = AXIS2_PLACEMENT_3D('',#11199,#7926,#7927) ;
#6334 = AXIS2_PLACEMENT_3D('',#11201,#7928,#7929) ;
#6335 = AXIS2_PLACEMENT_3D('',#11202,#7930,#7931) ;
#6336 = AXIS2_PLACEMENT_3D('',#11204,#7932,#7933) ;
#6337 = AXIS2_PLACEMENT_3D('',#11206,#7935,#7936) ;
#6338 = AXIS2_PLACEMENT_3D('',#11207,#7937,#7938) ;
#6339 = AXIS2_PLACEMENT_3D('',#11208,#7939,#7940) ;
#6340 = AXIS2_PLACEMENT_3D('',#11211,#7941,#7942) ;
#6341 = AXIS2_PLACEMENT_3D('',#11215,#7944,#7945) ;
#6342 = AXIS2_PLACEMENT_3D('',#11217,#7947,#7948) ;
#6343 = AXIS2_PLACEMENT_3D('',#11223,#7952,#7953) ;
#6344 = AXIS2_PLACEMENT_3D('',#11229,#7957,#7958) ;
#6345 = AXIS2_PLACEMENT_3D('',#11231,#7959,#7960) ;
#6346 = AXIS2_PLACEMENT_3D('',#11233,#7961,#7962) ;
#6347 = AXIS2_PLACEMENT_3D('',#11235,#7964,#7965) ;
#6348 = AXIS2_PLACEMENT_3D('',#11241,#7969,#7970) ;
#6349 = AXIS2_PLACEMENT_3D('',#11243,#7971,#7972) ;
#6350 = AXIS2_PLACEMENT_3D('',#11245,#7973,#7974) ;
#6351 = AXIS2_PLACEMENT_3D('',#11247,#7976,#7977) ;
#6352 = AXIS2_PLACEMENT_3D('',#11249,#7978,#7979) ;
#6353 = AXIS2_PLACEMENT_3D('',#11251,#7980,#7981) ;
#6354 = AXIS2_PLACEMENT_3D('',#11253,#7983,#7984) ;
#6355 = AXIS2_PLACEMENT_3D('',#11256,#7987,#7988) ;
#6356 = AXIS2_PLACEMENT_3D('',#11257,#7989,#7990) ;
#6357 = AXIS2_PLACEMENT_3D('',#11258,#7991,#7992) ;
#6358 = AXIS2_PLACEMENT_3D('',#11259,#7993,#7994) ;
#6359 = AXIS2_PLACEMENT_3D('',#11261,#7995,#7996) ;
#6360 = AXIS2_PLACEMENT_3D('',#11264,#7998,#7999) ;
#6361 = AXIS2_PLACEMENT_3D('',#11265,#8000,#8001) ;
#6362 = AXIS2_PLACEMENT_3D('',#11268,#8002,#8003) ;
#6363 = AXIS2_PLACEMENT_3D('',#11272,#8005,#8006) ;
#6364 = AXIS2_PLACEMENT_3D('',#11274,#8008,#8009) ;
#6365 = AXIS2_PLACEMENT_3D('',#11280,#8013,#8014) ;
#6366 = AXIS2_PLACEMENT_3D('',#11282,#8015,#8016) ;
#6367 = AXIS2_PLACEMENT_3D('',#11284,#8017,#8018) ;
#6368 = AXIS2_PLACEMENT_3D('',#11286,#8020,#8021) ;
#6369 = AXIS2_PLACEMENT_3D('',#11288,#8022,#8023) ;
#6370 = AXIS2_PLACEMENT_3D('',#11290,#8024,#8025) ;
#6371 = AXIS2_PLACEMENT_3D('',#11292,#8027,#8028) ;
#6372 = AXIS2_PLACEMENT_3D('',#11298,#8032,#8033) ;
#6373 = AXIS2_PLACEMENT_3D('',#11300,#8034,#8035) ;
#6374 = AXIS2_PLACEMENT_3D('',#11302,#8036,#8037) ;
#6375 = AXIS2_PLACEMENT_3D('',#11304,#8039,#8040) ;
#6376 = AXIS2_PLACEMENT_3D('',#11310,#8044,#8045) ;
#6377 = AXIS2_PLACEMENT_3D('',#11312,#8046,#8047) ;
#6378 = AXIS2_PLACEMENT_3D('',#11314,#8048,#8049) ;
#6379 = AXIS2_PLACEMENT_3D('',#11316,#8051,#8052) ;
#6380 = AXIS2_PLACEMENT_3D('',#11318,#8053,#8054) ;
#6381 = AXIS2_PLACEMENT_3D('',#11320,#8055,#8056) ;
#6382 = AXIS2_PLACEMENT_3D('',#11322,#8058,#8059) ;
#6383 = AXIS2_PLACEMENT_3D('',#11325,#8062,#8063) ;
#6384 = AXIS2_PLACEMENT_3D('',#11326,#8064,#8065) ;
#6385 = AXIS2_PLACEMENT_3D('',#11327,#8066,#8067) ;
#6386 = AXIS2_PLACEMENT_3D('',#11328,#8068,#8069) ;
#6387 = AXIS2_PLACEMENT_3D('',#11330,#8070,#8071) ;
#6388 = AXIS2_PLACEMENT_3D('',#11333,#8073,#8074) ;
#6389 = AXIS2_PLACEMENT_3D('',#11334,#8075,#8076) ;
#6390 = AXIS2_PLACEMENT_3D('',#11336,#8077,#8078) ;
#6391 = AXIS2_PLACEMENT_3D('',#11337,#8079,#8080) ;
#6392 = AXIS2_PLACEMENT_3D('',#11339,#8081,#8082) ;
#6393 = AXIS2_PLACEMENT_3D('',#11341,#8084,#8085) ;
#6394 = AXIS2_PLACEMENT_3D('',#11342,#8086,#8087) ;
#6395 = AXIS2_PLACEMENT_3D('',#11343,#8088,#8089) ;
#6396 = AXIS2_PLACEMENT_3D('',#11344,#8090,#8091) ;
#6397 = AXIS2_PLACEMENT_3D('',#11345,#8092,#8093) ;
#6398 = AXIS2_PLACEMENT_3D('',#11346,#8094,#8095) ;
#6399 = AXIS2_PLACEMENT_3D('',#11347,#8096,#8097) ;
#6400 = AXIS2_PLACEMENT_3D('',#11348,#8098,#8099) ;
#6401 = AXIS2_PLACEMENT_3D('',#11349,#8100,#8101) ;
#6402 = AXIS2_PLACEMENT_3D('',#11350,#8102,#8103) ;
#6403 = AXIS2_PLACEMENT_3D('',#11351,#8104,#8105) ;
#6404 = AXIS2_PLACEMENT_3D('',#11352,#8106,#8107) ;
#6405 = AXIS2_PLACEMENT_3D('',#11353,#8108,#8109) ;
#6406 = AXIS2_PLACEMENT_3D('',#11354,#8110,#8111) ;
#6407 = AXIS2_PLACEMENT_3D('',#11355,#8112,#8113) ;
#6408 = AXIS2_PLACEMENT_3D('',#11356,#8114,#8115) ;
#6409 = AXIS2_PLACEMENT_3D('',#11357,#8116,#8117) ;
#6410 = AXIS2_PLACEMENT_3D('',#11358,#8118,#8119) ;
#6411 = AXIS2_PLACEMENT_3D('',#11359,#8120,#8121) ;
#6412 = AXIS2_PLACEMENT_3D('',#11360,#8122,#8123) ;
#6413 = AXIS2_PLACEMENT_3D('',#11361,#8124,#8125) ;
#6414 = AXIS2_PLACEMENT_3D('',#11362,#8126,#8127) ;
#6415 = DIRECTION('axis',(0.,0.,1.)) ;
#6416 = DIRECTION('refdir',(1.,0.,0.)) ;
#6417 = DIRECTION('axis',(0.,0.,1.)) ;
#6418 = DIRECTION('refdir',(1.,0.,0.)) ;
#6419 = DIRECTION('center_axis',(0.,0.,1.)) ;
#6420 = DIRECTION('ref_axis',(1.,0.,0.)) ;
#6421 = DIRECTION('center_axis',(0.,0.,1.)) ;
#6422 = DIRECTION('ref_axis',(1.,0.,0.)) ;
#6423 = DIRECTION('',(0.,0.,1.)) ;
#6424 = DIRECTION('center_axis',(0.,0.,-1.)) ;
#6425 = DIRECTION('ref_axis',(1.,0.,0.)) ;
#6426 = DIRECTION('center_axis',(1.,0.,0.)) ;
#6427 = DIRECTION('ref_axis',(0.,0.,-1.)) ;
#6428 = DIRECTION('center_axis',(1.,0.,0.)) ;
#6429 = DIRECTION('ref_axis',(0.,0.,-1.)) ;
#6430 = DIRECTION('',(1.,0.,0.)) ;
#6431 = DIRECTION('center_axis',(-1.,0.,0.)) ;
#6432 = DIRECTION('ref_axis',(0.,0.,-1.)) ;
#6433 = DIRECTION('center_axis',(1.,0.,0.)) ;
#6434 = DIRECTION('ref_axis',(0.,0.,-1.)) ;
#6435 = DIRECTION('center_axis',(1.,0.,0.)) ;
#6436 = DIRECTION('ref_axis',(0.,0.,-1.)) ;
#6437 = DIRECTION('',(1.,0.,0.)) ;
#6438 = DIRECTION('center_axis',(-1.,0.,0.)) ;
#6439 = DIRECTION('ref_axis',(0.,0.,-1.)) ;
#6440 = DIRECTION('center_axis',(0.,1.,0.)) ;
#6441 = DIRECTION('ref_axis',(0.,0.,1.)) ;
#6442 = DIRECTION('center_axis',(0.,1.,0.)) ;
#6443 = DIRECTION('ref_axis',(1.67369913353994E-16,0.,1.)) ;
#6444 = DIRECTION('',(0.,0.,1.)) ;
#6445 = DIRECTION('',(1.,0.,0.)) ;
#6446 = DIRECTION('',(0.,0.,1.)) ;
#6447 = DIRECTION('center_axis',(0.,1.,0.)) ;
#6448 = DIRECTION('ref_axis',(-2.23159884471991E-16,-3.94494668997379E-17,
1.)) ;
#6449 = DIRECTION('',(1.,0.,0.)) ;
#6450 = DIRECTION('center_axis',(1.,0.,0.)) ;
#6451 = DIRECTION('ref_axis',(0.,0.,-1.)) ;
#6452 = DIRECTION('',(0.,-0.638189460570586,0.769879349259755)) ;
#6453 = DIRECTION('',(0.,0.193633031896661,0.981074028276412)) ;
#6454 = DIRECTION('',(0.,0.289220322623654,0.957262558017114)) ;
#6455 = DIRECTION('',(0.,1.,0.)) ;
#6456 = DIRECTION('',(0.,0.,-1.)) ;
#6457 = DIRECTION('',(0.,-1.,0.)) ;
#6458 = DIRECTION('',(0.,-0.989949493661166,0.141421356237312)) ;
#6459 = DIRECTION('center_axis',(0.,0.981074028276412,-0.193633031896661)) ;
#6460 = DIRECTION('ref_axis',(0.,0.193633031896661,0.981074028276412)) ;
#6461 = DIRECTION('',(0.,0.193633031896661,0.981074028276412)) ;
#6462 = DIRECTION('',(1.,0.,0.)) ;
#6463 = DIRECTION('center_axis',(0.,0.957262558017114,-0.289220322623654)) ;
#6464 = DIRECTION('ref_axis',(0.,0.289220322623654,0.957262558017114)) ;
#6465 = DIRECTION('',(0.,0.289220322623654,0.957262558017114)) ;
#6466 = DIRECTION('',(1.,0.,0.)) ;
#6467 = DIRECTION('center_axis',(0.,0.,-1.)) ;
#6468 = DIRECTION('ref_axis',(0.,1.,0.)) ;
#6469 = DIRECTION('',(0.,1.,0.)) ;
#6470 = DIRECTION('',(1.,0.,0.)) ;
#6471 = DIRECTION('center_axis',(0.,-1.,0.)) ;
#6472 = DIRECTION('ref_axis',(0.,0.,-1.)) ;
#6473 = DIRECTION('',(-1.,0.,0.)) ;
#6474 = DIRECTION('',(0.,0.,-1.)) ;
#6475 = DIRECTION('center_axis',(1.,0.,0.)) ;
#6476 = DIRECTION('ref_axis',(0.,0.,-1.)) ;
#6477 = DIRECTION('',(0.,0.638189460570586,-0.769879349259755)) ;
#6478 = DIRECTION('',(0.,0.989949493661166,-0.141421356237312)) ;
#6479 = DIRECTION('',(0.,1.,0.)) ;
#6480 = DIRECTION('center_axis',(0.,0.769879349259756,0.638189460570586)) ;
#6481 = DIRECTION('ref_axis',(0.,-0.638189460570586,0.769879349259755)) ;
#6482 = DIRECTION('',(0.,-0.638189460570586,0.769879349259755)) ;
#6483 = DIRECTION('',(1.,0.,0.)) ;
#6484 = DIRECTION('',(0.,0.638189460570586,-0.769879349259755)) ;
#6485 = DIRECTION('center_axis',(0.,-0.638189460570586,0.769879349259756)) ;
#6486 = DIRECTION('ref_axis',(0.707106781186548,0.54438690855706,0.451268095251245)) ;
#6487 = DIRECTION('center_axis',(0.,-0.141421356237312,-0.989949493661166)) ;
#6488 = DIRECTION('ref_axis',(0.,0.989949493661166,-0.141421356237312)) ;
#6489 = DIRECTION('center_axis',(1.39759027204558E-15,-0.039937225530417,
0.999202190758674)) ;
#6490 = DIRECTION('ref_axis',(0.,0.999202190758674,0.039937225530417)) ;
#6491 = DIRECTION('',(0.,0.638189460570586,-0.769879349259755)) ;
#6492 = DIRECTION('center_axis',(0.,-0.339205432400665,0.940712322992464)) ;
#6493 = DIRECTION('ref_axis',(0.,0.940712322992464,0.339205432400665)) ;
#6494 = DIRECTION('center_axis',(0.,0.141421356237312,0.989949493661166)) ;
#6495 = DIRECTION('ref_axis',(0.,-0.989949493661166,0.141421356237312)) ;
#6496 = DIRECTION('',(1.,0.,0.)) ;
#6497 = DIRECTION('center_axis',(0.,-1.,0.)) ;
#6498 = DIRECTION('ref_axis',(0.,0.,-1.)) ;
#6499 = DIRECTION('center_axis',(-1.,0.,0.)) ;
#6500 = DIRECTION('ref_axis',(0.,1.,0.)) ;
#6501 = DIRECTION('center_axis',(0.,-1.,0.)) ;
#6502 = DIRECTION('ref_axis',(-1.,0.,0.)) ;
#6503 = DIRECTION('center_axis',(-1.,0.,0.)) ;
#6504 = DIRECTION('ref_axis',(0.,0.,1.)) ;
#6505 = DIRECTION('center_axis',(0.,1.,0.)) ;
#6506 = DIRECTION('ref_axis',(-1.,0.,0.)) ;
#6507 = DIRECTION('center_axis',(1.,0.,0.)) ;
#6508 = DIRECTION('ref_axis',(0.,0.707106781186549,0.707106781186546)) ;
#6509 = DIRECTION('center_axis',(-1.,0.,0.)) ;
#6510 = DIRECTION('ref_axis',(0.,0.,1.)) ;
#6511 = DIRECTION('',(-1.,0.,0.)) ;
#6512 = DIRECTION('',(1.,0.,0.)) ;
#6513 = DIRECTION('center_axis',(0.,-1.,0.)) ;
#6514 = DIRECTION('ref_axis',(0.,0.,-1.)) ;
#6515 = DIRECTION('center_axis',(1.,0.,0.)) ;
#6516 = DIRECTION('ref_axis',(0.,0.,-1.)) ;
#6517 = DIRECTION('center_axis',(0.,1.,0.)) ;
#6518 = DIRECTION('ref_axis',(1.,0.,0.)) ;
#6519 = DIRECTION('center_axis',(0.,-1.,0.)) ;
#6520 = DIRECTION('ref_axis',(1.,0.,0.)) ;
#6521 = DIRECTION('center_axis',(-1.,0.,0.)) ;
#6522 = DIRECTION('ref_axis',(0.,0.707106781186549,-0.707106781186546)) ;
#6523 = DIRECTION('',(1.,0.,0.)) ;
#6524 = DIRECTION('',(-1.,0.,0.)) ;
#6525 = DIRECTION('center_axis',(0.,0.,1.)) ;
#6526 = DIRECTION('ref_axis',(1.,0.,0.)) ;
#6527 = DIRECTION('',(0.,1.,0.)) ;
#6528 = DIRECTION('',(1.,0.,0.)) ;
#6529 = DIRECTION('',(0.,1.,0.)) ;
#6530 = DIRECTION('center_axis',(0.,1.,0.)) ;
#6531 = DIRECTION('ref_axis',(0.,0.,-1.)) ;
#6532 = DIRECTION('',(0.,1.,0.)) ;
#6533 = DIRECTION('center_axis',(0.,-1.,0.)) ;
#6534 = DIRECTION('ref_axis',(0.,0.,-1.)) ;
#6535 = DIRECTION('center_axis',(0.,1.,0.)) ;
#6536 = DIRECTION('ref_axis',(1.,0.,0.)) ;
#6537 = DIRECTION('center_axis',(0.,-1.,0.)) ;
#6538 = DIRECTION('ref_axis',(-0.677879474603844,0.,-0.735173053036369)) ;
#6539 = DIRECTION('',(0.707106781186548,0.,-0.707106781186547)) ;
#6540 = DIRECTION('center_axis',(0.,-1.,0.)) ;
#6541 = DIRECTION('ref_axis',(-0.921249561411385,0.,-0.388972037040364)) ;
#6542 = DIRECTION('',(0.,0.,-1.)) ;
#6543 = DIRECTION('',(-1.,0.,0.)) ;
#6544 = DIRECTION('',(0.,0.,1.)) ;
#6545 = DIRECTION('center_axis',(0.,1.,0.)) ;
#6546 = DIRECTION('ref_axis',(1.,0.,0.)) ;
#6547 = DIRECTION('center_axis',(0.,-1.,0.)) ;
#6548 = DIRECTION('ref_axis',(0.,0.,-1.)) ;
#6549 = DIRECTION('center_axis',(-1.,0.,0.)) ;
#6550 = DIRECTION('ref_axis',(0.,0.,1.)) ;
#6551 = DIRECTION('center_axis',(0.,-1.,0.)) ;
#6552 = DIRECTION('ref_axis',(1.,0.,0.)) ;
#6553 = DIRECTION('center_axis',(0.,-1.,0.)) ;
#6554 = DIRECTION('ref_axis',(1.,0.,0.)) ;
#6555 = DIRECTION('center_axis',(0.,1.,0.)) ;
#6556 = DIRECTION('ref_axis',(1.,0.,0.)) ;
#6557 = DIRECTION('',(0.,-1.,0.)) ;
#6558 = DIRECTION('center_axis',(0.,-1.,0.)) ;
#6559 = DIRECTION('ref_axis',(1.,0.,0.)) ;
#6560 = DIRECTION('center_axis',(0.,-1.,0.)) ;
#6561 = DIRECTION('ref_axis',(0.,0.,-1.)) ;
#6562 = DIRECTION('center_axis',(0.,1.,0.)) ;
#6563 = DIRECTION('ref_axis',(1.,0.,0.)) ;
#6564 = DIRECTION('center_axis',(-1.,0.,0.)) ;
#6565 = DIRECTION('ref_axis',(0.,0.,1.)) ;
#6566 = DIRECTION('center_axis',(0.,-1.,0.)) ;
#6567 = DIRECTION('ref_axis',(1.,0.,0.)) ;
#6568 = DIRECTION('center_axis',(0.,-1.,0.)) ;
#6569 = DIRECTION('ref_axis',(1.,0.,0.)) ;
#6570 = DIRECTION('center_axis',(0.,1.,0.)) ;
#6571 = DIRECTION('ref_axis',(1.,0.,0.)) ;
#6572 = DIRECTION('',(-1.,0.,0.)) ;
#6573 = DIRECTION('',(0.,0.,1.)) ;
#6574 = DIRECTION('center_axis',(0.,-1.,0.)) ;
#6575 = DIRECTION('ref_axis',(0.921249561411385,0.,-0.388972037040363)) ;
#6576 = DIRECTION('',(0.707106781186548,0.,0.707106781186547)) ;
#6577 = DIRECTION('center_axis',(0.,-1.,0.)) ;
#6578 = DIRECTION('ref_axis',(0.677879474603844,0.,-0.735173053036369)) ;
#6579 = DIRECTION('',(0.,0.,-1.)) ;
#6580 = DIRECTION('center_axis',(0.,1.,0.)) ;
#6581 = DIRECTION('ref_axis',(-1.,0.,0.)) ;
#6582 = DIRECTION('',(-1.,0.,0.)) ;
#6583 = DIRECTION('center_axis',(0.,1.,0.)) ;
#6584 = DIRECTION('ref_axis',(1.,0.,0.)) ;
#6585 = DIRECTION('',(1.,0.,0.)) ;
#6586 = DIRECTION('center_axis',(0.,1.,0.)) ;
#6587 = DIRECTION('ref_axis',(1.,0.,0.)) ;
#6588 = DIRECTION('',(0.,-1.,0.)) ;
#6589 = DIRECTION('center_axis',(0.,-1.,0.)) ;
#6590 = DIRECTION('ref_axis',(1.,0.,0.)) ;
#6591 = DIRECTION('center_axis',(0.,-1.,0.)) ;
#6592 = DIRECTION('ref_axis',(0.,0.,-1.)) ;
#6593 = DIRECTION('center_axis',(-1.,0.,0.)) ;
#6594 = DIRECTION('ref_axis',(0.,1.,0.)) ;
#6595 = DIRECTION('center_axis',(0.,-1.,0.)) ;
#6596 = DIRECTION('ref_axis',(-1.,0.,0.)) ;
#6597 = DIRECTION('center_axis',(-1.,0.,0.)) ;
#6598 = DIRECTION('ref_axis',(0.,0.,1.)) ;
#6599 = DIRECTION('center_axis',(1.,0.,0.)) ;
#6600 = DIRECTION('ref_axis',(0.,0.707106781186549,0.707106781186546)) ;
#6601 = DIRECTION('center_axis',(-1.,0.,0.)) ;
#6602 = DIRECTION('ref_axis',(0.,0.,1.)) ;
#6603 = DIRECTION('',(1.,0.,0.)) ;
#6604 = DIRECTION('center_axis',(0.,-1.,0.)) ;
#6605 = DIRECTION('ref_axis',(0.,0.,-1.)) ;
#6606 = DIRECTION('center_axis',(1.,0.,0.)) ;
#6607 = DIRECTION('ref_axis',(0.,0.,-1.)) ;
#6608 = DIRECTION('center_axis',(0.,-1.,0.)) ;
#6609 = DIRECTION('ref_axis',(1.,0.,0.)) ;
#6610 = DIRECTION('center_axis',(-1.,0.,0.)) ;
#6611 = DIRECTION('ref_axis',(0.,0.707106781186549,-0.707106781186546)) ;
#6612 = DIRECTION('',(-1.,0.,0.)) ;
#6613 = DIRECTION('center_axis',(0.,0.,1.)) ;
#6614 = DIRECTION('ref_axis',(1.,0.,0.)) ;
#6615 = DIRECTION('',(0.,1.,0.)) ;
#6616 = DIRECTION('',(1.,0.,0.)) ;
#6617 = DIRECTION('',(0.,1.,0.)) ;
#6618 = DIRECTION('center_axis',(0.,1.,0.)) ;
#6619 = DIRECTION('ref_axis',(0.,0.,-1.)) ;
#6620 = DIRECTION('',(0.,1.,0.)) ;
#6621 = DIRECTION('center_axis',(0.,-1.,0.)) ;
#6622 = DIRECTION('ref_axis',(0.,0.,-1.)) ;
#6623 = DIRECTION('center_axis',(0.,0.,-1.)) ;
#6624 = DIRECTION('ref_axis',(0.,1.,0.)) ;
#6625 = DIRECTION('center_axis',(0.,1.,0.)) ;
#6626 = DIRECTION('ref_axis',(0.,0.,1.)) ;
#6627 = DIRECTION('center_axis',(0.,-1.,0.)) ;
#6628 = DIRECTION('ref_axis',(0.707106781186544,0.,0.707106781186551)) ;
#6629 = DIRECTION('center_axis',(0.,1.,0.)) ;
#6630 = DIRECTION('ref_axis',(0.,0.,1.)) ;
#6631 = DIRECTION('',(0.,1.,0.)) ;
#6632 = DIRECTION('',(0.,-1.,0.)) ;
#6633 = DIRECTION('center_axis',(1.,0.,0.)) ;
#6634 = DIRECTION('ref_axis',(0.,0.707106781186543,0.707106781186552)) ;
#6635 = DIRECTION('center_axis',(1.,0.,0.)) ;
#6636 = DIRECTION('ref_axis',(0.,1.,0.)) ;
#6637 = DIRECTION('',(1.,0.,0.)) ;
#6638 = DIRECTION('center_axis',(-1.,0.,0.)) ;
#6639 = DIRECTION('ref_axis',(0.,0.,1.)) ;
#6640 = DIRECTION('center_axis',(0.,0.,1.)) ;
#6641 = DIRECTION('ref_axis',(1.,0.,0.)) ;
#6642 = DIRECTION('center_axis',(0.,0.,-1.)) ;
#6643 = DIRECTION('ref_axis',(-0.707106781186547,-0.707106781186548,0.)) ;
#6644 = DIRECTION('center_axis',(0.,0.,1.)) ;
#6645 = DIRECTION('ref_axis',(-0.707106781186547,-0.707106781186548,0.)) ;
#6646 = DIRECTION('center_axis',(0.,1.,0.)) ;
#6647 = DIRECTION('ref_axis',(0.,0.,1.)) ;
#6648 = DIRECTION('center_axis',(0.,1.,0.)) ;
#6649 = DIRECTION('ref_axis',(0.921249561411386,0.,-0.388972037040363)) ;
#6650 = DIRECTION('center_axis',(0.,1.,0.)) ;
#6651 = DIRECTION('ref_axis',(0.,0.,1.)) ;
#6652 = DIRECTION('center_axis',(0.,1.,0.)) ;
#6653 = DIRECTION('ref_axis',(-0.921249561411385,0.,-0.388972037040364)) ;
#6654 = DIRECTION('center_axis',(-0.707106781186548,0.,0.707106781186547)) ;
#6655 = DIRECTION('ref_axis',(-0.499999999999999,0.707106781186549,-0.499999999999999)) ;
#6656 = DIRECTION('',(-0.707106781186548,0.,0.707106781186547)) ;
#6657 = DIRECTION('center_axis',(-0.751890603952275,6.67813008405704E-15,
-0.659287888322153)) ;
#6658 = DIRECTION('ref_axis',(8.88178419700124E-15,1.,0.)) ;
#6659 = DIRECTION('center_axis',(-0.791256109639887,-1.01273265766357E-13,
0.611484888576612)) ;
#6660 = DIRECTION('ref_axis',(-4.44089209850062E-15,1.,1.59872115546022E-13)) ;
#6661 = DIRECTION('center_axis',(0.,1.,0.)) ;
#6662 = DIRECTION('ref_axis',(2.78699993901511E-15,0.,-1.)) ;
#6663 = DIRECTION('center_axis',(-0.79125610963988,0.,-0.61148488857662)) ;
#6664 = DIRECTION('ref_axis',(0.,1.,0.)) ;
#6665 = DIRECTION('center_axis',(0.,1.,0.)) ;
#6666 = DIRECTION('ref_axis',(6.69381353752835E-17,0.,-1.)) ;
#6667 = DIRECTION('center_axis',(0.,-1.,0.)) ;
#6668 = DIRECTION('ref_axis',(6.69381353752835E-17,0.,-1.)) ;
#6669 = DIRECTION('center_axis',(0.,1.,0.)) ;
#6670 = DIRECTION('ref_axis',(0.,0.,1.)) ;
#6671 = DIRECTION('center_axis',(-0.751890603952276,-5.03317541149096E-15,
0.659287888322151)) ;
#6672 = DIRECTION('ref_axis',(8.88178419700124E-15,1.,1.77635683940025E-14)) ;
#6673 = DIRECTION('center_axis',(0.,1.,0.)) ;
#6674 = DIRECTION('ref_axis',(-0.677879474603844,0.,-0.735173053036369)) ;
#6675 = DIRECTION('center_axis',(0.,1.,0.)) ;
#6676 = DIRECTION('ref_axis',(0.,0.,1.)) ;
#6677 = DIRECTION('center_axis',(0.,1.,0.)) ;
#6678 = DIRECTION('ref_axis',(0.677879474603844,0.,-0.735173053036369)) ;
#6679 = DIRECTION('center_axis',(-0.707106781186548,0.,-0.707106781186547)) ;
#6680 = DIRECTION('ref_axis',(0.499999999999999,0.707106781186549,-0.499999999999999)) ;
#6681 = DIRECTION('',(-0.707106781186548,0.,-0.707106781186547)) ;
#6682 = DIRECTION('center_axis',(0.,0.,1.)) ;
#6683 = DIRECTION('ref_axis',(-0.707106781186552,0.707106781186543,0.)) ;
#6684 = DIRECTION('',(0.,0.,1.)) ;
#6685 = DIRECTION('center_axis',(0.,0.,-1.)) ;
#6686 = DIRECTION('ref_axis',(-1.,0.,0.)) ;
#6687 = DIRECTION('center_axis',(0.,0.,-1.)) ;
#6688 = DIRECTION('ref_axis',(0.707106781186552,0.707106781186543,0.)) ;
#6689 = DIRECTION('center_axis',(0.,0.,-1.)) ;
#6690 = DIRECTION('ref_axis',(0.,1.,0.)) ;
#6691 = DIRECTION('',(0.,0.,-1.)) ;
#6692 = DIRECTION('center_axis',(1.,0.,0.)) ;
#6693 = DIRECTION('ref_axis',(0.,0.707106781186543,0.707106781186552)) ;
#6694 = DIRECTION('center_axis',(1.,0.,0.)) ;
#6695 = DIRECTION('ref_axis',(0.,1.,0.)) ;
#6696 = DIRECTION('',(1.,0.,0.)) ;
#6697 = DIRECTION('center_axis',(-1.,0.,0.)) ;
#6698 = DIRECTION('ref_axis',(0.,0.,1.)) ;
#6699 = DIRECTION('center_axis',(0.,0.,1.)) ;
#6700 = DIRECTION('ref_axis',(1.,0.,0.)) ;
#6701 = DIRECTION('center_axis',(0.,-1.,0.)) ;
#6702 = DIRECTION('ref_axis',(0.,0.,1.)) ;
#6703 = DIRECTION('center_axis',(0.,0.,-1.)) ;
#6704 = DIRECTION('ref_axis',(0.707106781186547,-0.707106781186548,0.)) ;
#6705 = DIRECTION('center_axis',(0.,0.,1.)) ;
#6706 = DIRECTION('ref_axis',(0.707106781186547,-0.707106781186548,0.)) ;
#6707 = DIRECTION('center_axis',(0.,-1.,0.)) ;
#6708 = DIRECTION('ref_axis',(-0.707106781186541,0.,0.707106781186554)) ;
#6709 = DIRECTION('center_axis',(0.,-1.,0.)) ;
#6710 = DIRECTION('ref_axis',(0.,0.,1.)) ;
#6711 = DIRECTION('',(0.,-1.,0.)) ;
#6712 = DIRECTION('',(0.,1.,0.)) ;
#6713 = DIRECTION('center_axis',(0.,-0.039937225530417,0.999202190758674)) ;
#6714 = DIRECTION('ref_axis',(0.,0.999202190758674,0.039937225530417)) ;
#6715 = DIRECTION('center_axis',(0.,0.,-1.)) ;
#6716 = DIRECTION('ref_axis',(1.46109022176344E-16,1.,0.)) ;
#6717 = DIRECTION('center_axis',(-0.816496580927738,-0.408248290463869,-0.408248290463833)) ;
#6718 = DIRECTION('ref_axis',(-0.577350269189608,0.577350269189647,0.577350269189622)) ;
#6719 = DIRECTION('center_axis',(0.,1.,0.)) ;
#6720 = DIRECTION('ref_axis',(-1.,0.,-1.77635683940029E-14)) ;
#6721 = DIRECTION('center_axis',(-0.816496580927738,0.408248290463869,0.408248290463833)) ;
#6722 = DIRECTION('ref_axis',(0.577350269189608,0.577350269189647,0.577350269189622)) ;
#6723 = DIRECTION('center_axis',(0.,1.,0.)) ;
#6724 = DIRECTION('ref_axis',(-1.77635683940029E-14,0.,1.)) ;
#6725 = DIRECTION('center_axis',(1.,0.,0.)) ;
#6726 = DIRECTION('ref_axis',(0.,0.,-1.)) ;
#6727 = DIRECTION('',(0.,0.,1.)) ;
#6728 = DIRECTION('',(0.,1.,0.)) ;
#6729 = DIRECTION('',(0.,-0.287347885566346,-0.957826285221151)) ;
#6730 = DIRECTION('center_axis',(-1.,0.,0.)) ;
#6731 = DIRECTION('ref_axis',(0.,0.988836773758751,-0.14900280152529)) ;
#6732 = DIRECTION('',(0.,0.,-1.)) ;
#6733 = DIRECTION('center_axis',(0.,0.,1.)) ;
#6734 = DIRECTION('ref_axis',(-0.707106781186547,-0.707106781186548,0.)) ;
#6735 = DIRECTION('center_axis',(0.707106781186548,0.,0.707106781186547)) ;
#6736 = DIRECTION('ref_axis',(-0.707106781186547,0.,0.707106781186548)) ;
#6737 = DIRECTION('center_axis',(0.,1.,0.)) ;
#6738 = DIRECTION('ref_axis',(1.,0.,0.)) ;
#6739 = DIRECTION('',(-1.,0.,0.)) ;
#6740 = DIRECTION('center_axis',(1.,0.,0.)) ;
#6741 = DIRECTION('ref_axis',(0.,-0.707106781186546,0.707106781186549)) ;
#6742 = DIRECTION('center_axis',(-0.707106781186548,0.,0.707106781186547)) ;
#6743 = DIRECTION('ref_axis',(-0.707106781186547,0.,-0.707106781186548)) ;
#6744 = DIRECTION('',(1.,0.,0.)) ;
#6745 = DIRECTION('center_axis',(0.,0.,-1.)) ;
#6746 = DIRECTION('ref_axis',(0.707106781186547,-0.707106781186548,0.)) ;
#6747 = DIRECTION('',(0.,0.,-1.)) ;
#6748 = DIRECTION('center_axis',(1.,0.,0.)) ;
#6749 = DIRECTION('ref_axis',(0.,0.,-1.)) ;
#6750 = DIRECTION('',(0.,-0.638189460570586,0.769879349259755)) ;
#6751 = DIRECTION('',(0.,0.,1.)) ;
#6752 = DIRECTION('center_axis',(1.,0.,0.)) ;
#6753 = DIRECTION('ref_axis',(0.,0.988836773758751,-0.14900280152529)) ;
#6754 = DIRECTION('',(0.,0.287347885566346,0.957826285221151)) ;
#6755 = DIRECTION('',(0.,1.,0.)) ;
#6756 = DIRECTION('center_axis',(0.,-0.638189460570586,0.769879349259756)) ;
#6757 = DIRECTION('ref_axis',(-0.707106781186548,0.544386908557059,0.451268095251246)) ;
#6758 = DIRECTION('center_axis',(0.,0.339205432400664,-0.940712322992464)) ;
#6759 = DIRECTION('ref_axis',(0.,-0.940712322992464,-0.339205432400664)) ;
#6760 = DIRECTION('center_axis',(0.,-0.141421356237312,-0.989949493661166)) ;
#6761 = DIRECTION('ref_axis',(0.,0.989949493661166,-0.141421356237312)) ;
#6762 = DIRECTION('center_axis',(1.,0.,0.)) ;
#6763 = DIRECTION('ref_axis',(0.,0.,-1.)) ;
#6764 = DIRECTION('center_axis',(1.,0.,0.)) ;
#6765 = DIRECTION('ref_axis',(0.,0.988836773758751,-0.14900280152529)) ;
#6766 = DIRECTION('center_axis',(0.,0.,1.)) ;
#6767 = DIRECTION('ref_axis',(0.707106781186548,0.707106781186548,0.)) ;
#6768 = DIRECTION('',(0.,0.,1.)) ;
#6769 = DIRECTION('center_axis',(0.,0.287347885566346,0.957826285221151)) ;
#6770 = DIRECTION('ref_axis',(0.707106781186548,0.677285461478596,-0.203185638443579)) ;
#6771 = DIRECTION('center_axis',(0.,0.,1.)) ;
#6772 = DIRECTION('ref_axis',(-1.33971753756687E-15,1.,0.)) ;
#6773 = DIRECTION('',(0.,0.287347885566346,0.957826285221151)) ;
#6774 = DIRECTION('center_axis',(0.,0.141421356237312,0.989949493661166)) ;
#6775 = DIRECTION('ref_axis',(0.,-0.989949493661166,0.141421356237312)) ;
#6776 = DIRECTION('',(1.,0.,0.)) ;
#6777 = DIRECTION('center_axis',(0.,1.,0.)) ;
#6778 = DIRECTION('ref_axis',(0.,0.,1.)) ;
#6779 = DIRECTION('',(1.,0.,0.)) ;
#6780 = DIRECTION('',(0.,0.,-1.)) ;
#6781 = DIRECTION('center_axis',(1.,0.,0.)) ;
#6782 = DIRECTION('ref_axis',(0.,0.958771613297587,-0.284177749893868)) ;
#6783 = DIRECTION('',(1.,0.,0.)) ;
#6784 = DIRECTION('center_axis',(-1.,0.,0.)) ;
#6785 = DIRECTION('ref_axis',(0.,0.988836773758751,-0.14900280152529)) ;
#6786 = DIRECTION('center_axis',(0.,0.957826285221151,-0.287347885566346)) ;
#6787 = DIRECTION('ref_axis',(0.,0.287347885566346,0.957826285221151)) ;
#6788 = DIRECTION('',(1.,0.,0.)) ;
#6789 = DIRECTION('',(0.,-0.287347885566346,-0.957826285221151)) ;
#6790 = DIRECTION('center_axis',(1.,0.,0.)) ;
#6791 = DIRECTION('ref_axis',(0.,0.00800353445718605,-0.999967971205174)) ;
#6792 = DIRECTION('',(1.,0.,0.)) ;
#6793 = DIRECTION('center_axis',(0.,0.287347885566346,0.957826285221151)) ;
#6794 = DIRECTION('ref_axis',(-0.707106781186548,0.677285461478596,-0.203185638443579)) ;
#6795 = DIRECTION('center_axis',(0.,0.,1.)) ;
#6796 = DIRECTION('ref_axis',(1.33971753756687E-15,1.,0.)) ;
#6797 = DIRECTION('center_axis',(0.,0.,1.)) ;
#6798 = DIRECTION('ref_axis',(-0.707106781186548,0.707106781186548,0.)) ;
#6799 = DIRECTION('center_axis',(1.,0.,0.)) ;
#6800 = DIRECTION('ref_axis',(0.,0.,-1.)) ;
#6801 = DIRECTION('center_axis',(0.,0.,-1.)) ;
#6802 = DIRECTION('ref_axis',(0.,1.,0.)) ;
#6803 = DIRECTION('center_axis',(0.,0.,-1.)) ;
#6804 = DIRECTION('ref_axis',(-1.,0.,0.)) ;
#6805 = DIRECTION('',(0.,1.,0.)) ;
#6806 = DIRECTION('',(-1.,0.,0.)) ;
#6807 = DIRECTION('center_axis',(0.,1.,0.)) ;
#6808 = DIRECTION('ref_axis',(0.,0.,1.)) ;
#6809 = DIRECTION('center_axis',(0.,-1.,0.)) ;
#6810 = DIRECTION('ref_axis',(0.,0.,1.)) ;
#6811 = DIRECTION('center_axis',(0.,0.,-1.)) ;
#6812 = DIRECTION('ref_axis',(-1.,0.,0.)) ;
#6813 = DIRECTION('',(0.,1.,0.)) ;
#6814 = DIRECTION('',(-1.,0.,0.)) ;
#6815 = DIRECTION('center_axis',(0.,1.,0.)) ;
#6816 = DIRECTION('ref_axis',(0.,0.,1.)) ;
#6817 = DIRECTION('center_axis',(0.,-1.,0.)) ;
#6818 = DIRECTION('ref_axis',(0.,0.,1.)) ;
#6819 = DIRECTION('center_axis',(-1.,0.,0.)) ;
#6820 = DIRECTION('ref_axis',(0.,0.,1.)) ;
#6821 = DIRECTION('',(0.,1.,0.)) ;
#6822 = DIRECTION('',(0.,0.,-1.)) ;
#6823 = DIRECTION('',(0.,1.,0.)) ;
#6824 = DIRECTION('center_axis',(0.,1.,0.)) ;
#6825 = DIRECTION('ref_axis',(-0.692126626006242,0.,-0.721776096565421)) ;
#6826 = DIRECTION('',(0.,1.,0.)) ;
#6827 = DIRECTION('center_axis',(0.,1.,0.)) ;
#6828 = DIRECTION('ref_axis',(-0.692126626006242,0.,-0.721776096565421)) ;
#6829 = DIRECTION('center_axis',(-0.707106781186547,0.,-0.707106781186548)) ;
#6830 = DIRECTION('ref_axis',(-0.707106781186548,0.,0.707106781186547)) ;
#6831 = DIRECTION('',(0.,1.,0.)) ;
#6832 = DIRECTION('',(0.707106781186548,0.,-0.707106781186547)) ;
#6833 = DIRECTION('center_axis',(0.,1.,0.)) ;
#6834 = DIRECTION('ref_axis',(0.705422393987226,0.,-0.708787165559119)) ;
#6835 = DIRECTION('',(0.,1.,0.)) ;
#6836 = DIRECTION('center_axis',(0.,1.,0.)) ;
#6837 = DIRECTION('ref_axis',(0.705422393987226,0.,-0.708787165559119)) ;
#6838 = DIRECTION('center_axis',(0.707106781186547,0.,-0.707106781186548)) ;
#6839 = DIRECTION('ref_axis',(-0.707106781186548,0.,-0.707106781186547)) ;
#6840 = DIRECTION('',(0.,1.,0.)) ;
#6841 = DIRECTION('',(0.707106781186548,0.,0.707106781186547)) ;
#6842 = DIRECTION('center_axis',(0.,1.,0.)) ;
#6843 = DIRECTION('ref_axis',(0.999778380675594,0.,-0.0210520672069664)) ;
#6844 = DIRECTION('',(0.,1.,0.)) ;
#6845 = DIRECTION('center_axis',(0.,1.,0.)) ;
#6846 = DIRECTION('ref_axis',(0.999778380675594,0.,-0.0210520672069664)) ;
#6847 = DIRECTION('center_axis',(1.,0.,0.)) ;
#6848 = DIRECTION('ref_axis',(0.,0.,-1.)) ;
#6849 = DIRECTION('',(0.,1.,0.)) ;
#6850 = DIRECTION('',(0.,0.,1.)) ;
#6851 = DIRECTION('center_axis',(0.,1.,0.)) ;
#6852 = DIRECTION('ref_axis',(-1.77635683940029E-14,0.,1.)) ;
#6853 = DIRECTION('',(0.,1.,0.)) ;
#6854 = DIRECTION('center_axis',(0.,1.,0.)) ;
#6855 = DIRECTION('ref_axis',(-1.77635683940029E-14,0.,1.)) ;
#6856 = DIRECTION('center_axis',(0.,0.,1.)) ;
#6857 = DIRECTION('ref_axis',(1.,0.,0.)) ;
#6858 = DIRECTION('',(0.,1.,0.)) ;
#6859 = DIRECTION('',(-1.,0.,0.)) ;
#6860 = DIRECTION('center_axis',(0.,1.,0.)) ;
#6861 = DIRECTION('ref_axis',(-1.,0.,-1.77635683940029E-14)) ;
#6862 = DIRECTION('center_axis',(0.,1.,0.)) ;
#6863 = DIRECTION('ref_axis',(-1.,0.,-1.77635683940029E-14)) ;
#6864 = DIRECTION('center_axis',(0.,1.,0.)) ;
#6865 = DIRECTION('ref_axis',(1.,0.,0.)) ;
#6866 = DIRECTION('axis',(0.,0.,1.)) ;
#6867 = DIRECTION('refdir',(1.,0.,0.)) ;
#6868 = DIRECTION('center_axis',(0.,0.,-1.)) ;
#6869 = DIRECTION('ref_axis',(0.707106781186548,-0.707106781186548,0.)) ;
#6870 = DIRECTION('',(0.,0.,-1.)) ;
#6871 = DIRECTION('center_axis',(0.,0.,-1.)) ;
#6872 = DIRECTION('ref_axis',(1.,0.,0.)) ;
#6873 = DIRECTION('',(0.,0.,1.)) ;
#6874 = DIRECTION('center_axis',(0.707106781186554,0.,0.707106781186541)) ;
#6875 = DIRECTION('ref_axis',(0.707106781186541,0.,-0.707106781186554)) ;
#6876 = DIRECTION('center_axis',(-1.,0.,0.)) ;
#6877 = DIRECTION('ref_axis',(0.,0.,1.)) ;
#6878 = DIRECTION('center_axis',(1.,0.,0.)) ;
#6879 = DIRECTION('ref_axis',(0.,0.707106781186548,-0.707106781186548)) ;
#6880 = DIRECTION('center_axis',(-1.,0.,0.)) ;
#6881 = DIRECTION('ref_axis',(0.,0.707106781186548,-0.707106781186548)) ;
#6882 = DIRECTION('center_axis',(1.,0.,0.)) ;
#6883 = DIRECTION('ref_axis',(0.,0.,-1.)) ;
#6884 = DIRECTION('center_axis',(1.,0.,0.)) ;
#6885 = DIRECTION('ref_axis',(0.,-0.997759953305869,0.0668960057034024)) ;
#6886 = DIRECTION('',(0.,-0.969490981460344,0.245126981107871)) ;
#6887 = DIRECTION('center_axis',(1.,0.,0.)) ;
#6888 = DIRECTION('ref_axis',(0.,0.00361481447269016,-0.999993466536821)) ;
#6889 = DIRECTION('',(0.,1.,0.)) ;
#6890 = DIRECTION('center_axis',(1.,0.,0.)) ;
#6891 = DIRECTION('ref_axis',(0.,0.,-1.)) ;
#6892 = DIRECTION('center_axis',(1.,0.,0.)) ;
#6893 = DIRECTION('ref_axis',(0.,0.,-1.)) ;
#6894 = DIRECTION('center_axis',(0.,0.,1.)) ;
#6895 = DIRECTION('ref_axis',(-1.,0.,0.)) ;
#6896 = DIRECTION('center_axis',(-1.,0.,0.)) ;
#6897 = DIRECTION('ref_axis',(0.,0.707106781186548,-0.707106781186548)) ;
#6898 = DIRECTION('center_axis',(1.,0.,0.)) ;
#6899 = DIRECTION('ref_axis',(0.,0.707106781186548,-0.707106781186548)) ;
#6900 = DIRECTION('center_axis',(0.,0.,1.)) ;
#6901 = DIRECTION('ref_axis',(-0.707106781186548,-0.707106781186548,0.)) ;
#6902 = DIRECTION('center_axis',(-0.707106781186554,0.,0.707106781186541)) ;
#6903 = DIRECTION('ref_axis',(-0.707106781186541,0.,-0.707106781186554)) ;
#6904 = DIRECTION('',(0.,0.,-1.)) ;
#6905 = DIRECTION('',(0.,0.,1.)) ;
#6906 = DIRECTION('center_axis',(1.,0.,0.)) ;
#6907 = DIRECTION('ref_axis',(0.,0.,-1.)) ;
#6908 = DIRECTION('',(0.,1.,0.)) ;
#6909 = DIRECTION('center_axis',(1.,0.,0.)) ;
#6910 = DIRECTION('ref_axis',(0.,0.00361481447269016,-0.999993466536821)) ;
#6911 = DIRECTION('',(0.,-0.969490981460344,0.245126981107871)) ;
#6912 = DIRECTION('center_axis',(-1.,0.,0.)) ;
#6913 = DIRECTION('ref_axis',(0.,-0.997759953305869,0.0668960057034024)) ;
#6914 = DIRECTION('center_axis',(-1.,0.,0.)) ;
#6915 = DIRECTION('ref_axis',(0.,0.,-1.)) ;
#6916 = DIRECTION('center_axis',(0.,-1.,0.)) ;
#6917 = DIRECTION('ref_axis',(0.,0.,-1.)) ;
#6918 = DIRECTION('center_axis',(-1.,0.,0.)) ;
#6919 = DIRECTION('ref_axis',(0.,1.,0.)) ;
#6920 = DIRECTION('center_axis',(0.,-1.,0.)) ;
#6921 = DIRECTION('ref_axis',(-1.,0.,0.)) ;
#6922 = DIRECTION('center_axis',(-1.,0.,0.)) ;
#6923 = DIRECTION('ref_axis',(0.,0.,1.)) ;
#6924 = DIRECTION('center_axis',(0.,1.,0.)) ;
#6925 = DIRECTION('ref_axis',(-1.,0.,0.)) ;
#6926 = DIRECTION('center_axis',(1.,0.,0.)) ;
#6927 = DIRECTION('ref_axis',(0.,0.707106781186543,0.707106781186552)) ;
#6928 = DIRECTION('center_axis',(-1.,0.,0.)) ;
#6929 = DIRECTION('ref_axis',(0.,0.,1.)) ;
#6930 = DIRECTION('',(-1.,0.,0.)) ;
#6931 = DIRECTION('',(1.,0.,0.)) ;
#6932 = DIRECTION('center_axis',(0.,-1.,0.)) ;
#6933 = DIRECTION('ref_axis',(0.,0.,-1.)) ;
#6934 = DIRECTION('center_axis',(1.,0.,0.)) ;
#6935 = DIRECTION('ref_axis',(0.,0.,-1.)) ;
#6936 = DIRECTION('center_axis',(0.,1.,0.)) ;
#6937 = DIRECTION('ref_axis',(1.,0.,0.)) ;
#6938 = DIRECTION('center_axis',(0.,-1.,0.)) ;
#6939 = DIRECTION('ref_axis',(1.,0.,0.)) ;
#6940 = DIRECTION('center_axis',(-1.,0.,0.)) ;
#6941 = DIRECTION('ref_axis',(0.,0.707106781186543,-0.707106781186552)) ;
#6942 = DIRECTION('',(1.,0.,0.)) ;
#6943 = DIRECTION('',(-1.,0.,0.)) ;
#6944 = DIRECTION('center_axis',(0.,0.,1.)) ;
#6945 = DIRECTION('ref_axis',(1.,0.,0.)) ;
#6946 = DIRECTION('',(0.,1.,0.)) ;
#6947 = DIRECTION('',(1.,0.,0.)) ;
#6948 = DIRECTION('',(0.,1.,0.)) ;
#6949 = DIRECTION('center_axis',(0.,1.,0.)) ;
#6950 = DIRECTION('ref_axis',(-8.33188010975728E-16,0.,-1.)) ;
#6951 = DIRECTION('',(0.,1.,0.)) ;
#6952 = DIRECTION('center_axis',(0.,-1.,0.)) ;
#6953 = DIRECTION('ref_axis',(-8.33188010975728E-16,0.,-1.)) ;
#6954 = DIRECTION('center_axis',(0.,1.,0.)) ;
#6955 = DIRECTION('ref_axis',(1.,0.,0.)) ;
#6956 = DIRECTION('',(1.,0.,0.)) ;
#6957 = DIRECTION('center_axis',(0.,-1.,0.)) ;
#6958 = DIRECTION('ref_axis',(-0.707106781186544,0.,-0.707106781186551)) ;
#6959 = DIRECTION('',(0.,0.,-1.)) ;
#6960 = DIRECTION('center_axis',(0.,-1.,0.)) ;
#6961 = DIRECTION('ref_axis',(-0.846732995614247,0.,0.532018076890367)) ;
#6962 = DIRECTION('center_axis',(0.,-1.,0.)) ;
#6963 = DIRECTION('ref_axis',(4.71359210659789E-17,0.,1.)) ;
#6964 = DIRECTION('center_axis',(0.,-1.,0.)) ;
#6965 = DIRECTION('ref_axis',(0.846732995614246,0.,0.532018076890367)) ;
#6966 = DIRECTION('',(0.,0.,1.)) ;
#6967 = DIRECTION('center_axis',(0.,-1.,0.)) ;
#6968 = DIRECTION('ref_axis',(0.707106781186544,0.,-0.707106781186551)) ;
#6969 = DIRECTION('',(1.,0.,0.)) ;
#6970 = DIRECTION('',(1.,0.,0.)) ;
#6971 = DIRECTION('center_axis',(0.,1.,0.)) ;
#6972 = DIRECTION('ref_axis',(-1.,0.,0.)) ;
#6973 = DIRECTION('',(-1.,0.,0.)) ;
#6974 = DIRECTION('center_axis',(0.,1.,0.)) ;
#6975 = DIRECTION('ref_axis',(1.,0.,0.)) ;
#6976 = DIRECTION('',(1.,0.,0.)) ;
#6977 = DIRECTION('center_axis',(0.,-1.,0.)) ;
#6978 = DIRECTION('ref_axis',(0.,0.,-1.)) ;
#6979 = DIRECTION('center_axis',(-1.,0.,0.)) ;
#6980 = DIRECTION('ref_axis',(0.,1.,0.)) ;
#6981 = DIRECTION('center_axis',(0.,-1.,0.)) ;
#6982 = DIRECTION('ref_axis',(-1.,0.,0.)) ;
#6983 = DIRECTION('center_axis',(-1.,0.,0.)) ;
#6984 = DIRECTION('ref_axis',(0.,0.,1.)) ;
#6985 = DIRECTION('center_axis',(1.,0.,0.)) ;
#6986 = DIRECTION('ref_axis',(0.,0.707106781186543,0.707106781186552)) ;
#6987 = DIRECTION('center_axis',(-1.,0.,-8.88178419700113E-15)) ;
#6988 = DIRECTION('ref_axis',(-8.88178419700113E-15,0.,1.)) ;
#6989 = DIRECTION('',(1.,0.,0.)) ;
#6990 = DIRECTION('center_axis',(0.,-1.,0.)) ;
#6991 = DIRECTION('ref_axis',(0.,0.,-1.)) ;
#6992 = DIRECTION('center_axis',(1.,0.,0.)) ;
#6993 = DIRECTION('ref_axis',(0.,0.,-1.)) ;
#6994 = DIRECTION('center_axis',(0.,-1.,0.)) ;
#6995 = DIRECTION('ref_axis',(1.,0.,0.)) ;
#6996 = DIRECTION('center_axis',(-1.,0.,0.)) ;
#6997 = DIRECTION('ref_axis',(0.,0.707106781186543,-0.707106781186552)) ;
#6998 = DIRECTION('',(-1.,0.,0.)) ;
#6999 = DIRECTION('center_axis',(0.,0.,1.)) ;
#7000 = DIRECTION('ref_axis',(1.,0.,0.)) ;
#7001 = DIRECTION('',(0.,1.,0.)) ;
#7002 = DIRECTION('',(1.,0.,0.)) ;
#7003 = DIRECTION('',(0.,1.,0.)) ;
#7004 = DIRECTION('center_axis',(0.,1.,0.)) ;
#7005 = DIRECTION('ref_axis',(-8.33188010975728E-16,0.,-1.)) ;
#7006 = DIRECTION('',(0.,1.,0.)) ;
#7007 = DIRECTION('center_axis',(0.,-1.,0.)) ;
#7008 = DIRECTION('ref_axis',(-8.33188010975728E-16,0.,-1.)) ;
#7009 = DIRECTION('center_axis',(-1.,0.,0.)) ;
#7010 = DIRECTION('ref_axis',(0.,-0.99932673530985,-0.0366889096997627)) ;
#7011 = DIRECTION('',(-1.,0.,0.)) ;
#7012 = DIRECTION('center_axis',(1.,0.,0.)) ;
#7013 = DIRECTION('ref_axis',(0.,-0.997759953305869,0.0668960057034024)) ;
#7014 = DIRECTION('',(1.,0.,0.)) ;
#7015 = DIRECTION('center_axis',(0.,1.,0.)) ;
#7016 = DIRECTION('ref_axis',(0.,0.,1.)) ;
#7017 = DIRECTION('center_axis',(0.,1.,0.)) ;
#7018 = DIRECTION('ref_axis',(0.846732995614246,0.,0.532018076890367)) ;
#7019 = DIRECTION('center_axis',(0.,0.,-1.)) ;
#7020 = DIRECTION('ref_axis',(0.707106781186552,0.707106781186543,0.)) ;
#7021 = DIRECTION('',(0.,0.,-1.)) ;
#7022 = DIRECTION('center_axis',(0.,0.,1.)) ;
#7023 = DIRECTION('ref_axis',(1.,0.,0.)) ;
#7024 = DIRECTION('center_axis',(0.,1.,0.)) ;
#7025 = DIRECTION('ref_axis',(0.,0.,1.)) ;
#7026 = DIRECTION('center_axis',(1.,0.,0.)) ;
#7027 = DIRECTION('ref_axis',(0.,0.,-1.)) ;
#7028 = DIRECTION('center_axis',(0.,1.,0.)) ;
#7029 = DIRECTION('ref_axis',(0.707106781186544,0.,-0.707106781186551)) ;
#7030 = DIRECTION('center_axis',(-1.,0.,0.)) ;
#7031 = DIRECTION('ref_axis',(0.,0.707106781186555,-0.70710678118654)) ;
#7032 = DIRECTION('',(-1.,0.,0.)) ;
#7033 = DIRECTION('center_axis',(0.,1.,0.)) ;
#7034 = DIRECTION('ref_axis',(0.,0.,1.)) ;
#7035 = DIRECTION('center_axis',(0.,1.,0.)) ;
#7036 = DIRECTION('ref_axis',(-0.846732995614247,0.,0.532018076890367)) ;
#7037 = DIRECTION('center_axis',(-0.893020597138892,0.,-0.450015792040343)) ;
#7038 = DIRECTION('ref_axis',(-0.450015792040343,0.,0.893020597138892)) ;
#7039 = DIRECTION('center_axis',(0.,1.,0.)) ;
#7040 = DIRECTION('ref_axis',(0.,0.,1.)) ;
#7041 = DIRECTION('center_axis',(0.,1.,0.)) ;
#7042 = DIRECTION('ref_axis',(4.71359210659789E-17,0.,1.)) ;
#7043 = DIRECTION('center_axis',(-1.,0.,0.)) ;
#7044 = DIRECTION('ref_axis',(0.,0.707106781186555,-0.70710678118654)) ;
#7045 = DIRECTION('',(-1.,0.,0.)) ;
#7046 = DIRECTION('center_axis',(1.,0.,0.)) ;
#7047 = DIRECTION('ref_axis',(0.,0.,-1.)) ;
#7048 = DIRECTION('center_axis',(0.,1.,0.)) ;
#7049 = DIRECTION('ref_axis',(0.,0.,1.)) ;
#7050 = DIRECTION('center_axis',(0.,0.,-1.)) ;
#7051 = DIRECTION('ref_axis',(-1.,0.,0.)) ;
#7052 = DIRECTION('center_axis',(0.,1.,0.)) ;
#7053 = DIRECTION('ref_axis',(-0.707106781186544,0.,-0.707106781186551)) ;
#7054 = DIRECTION('center_axis',(0.,0.,1.)) ;
#7055 = DIRECTION('ref_axis',(-0.707106781186552,0.707106781186543,0.)) ;
#7056 = DIRECTION('',(0.,0.,1.)) ;
#7057 = DIRECTION('center_axis',(0.,0.,-1.)) ;
#7058 = DIRECTION('ref_axis',(-1.,0.,0.)) ;
#7059 = DIRECTION('',(0.,1.,0.)) ;
#7060 = DIRECTION('',(1.,0.,0.)) ;
#7061 = DIRECTION('',(0.,1.,0.)) ;
#7062 = DIRECTION('',(1.,0.,0.)) ;
#7063 = DIRECTION('center_axis',(0.,1.,0.)) ;
#7064 = DIRECTION('ref_axis',(1.,0.,-6.83214169000097E-15)) ;
#7065 = DIRECTION('',(0.,1.,0.)) ;
#7066 = DIRECTION('center_axis',(0.,1.,0.)) ;
#7067 = DIRECTION('ref_axis',(1.,0.,-6.83214169000097E-15)) ;
#7068 = DIRECTION('center_axis',(1.,0.,0.)) ;
#7069 = DIRECTION('ref_axis',(0.,0.,-1.)) ;
#7070 = DIRECTION('',(0.,1.,0.)) ;
#7071 = DIRECTION('',(0.,0.,1.)) ;
#7072 = DIRECTION('center_axis',(0.,1.,0.)) ;
#7073 = DIRECTION('ref_axis',(0.427975386405345,0.,0.903790389764793)) ;
#7074 = DIRECTION('',(0.,1.,0.)) ;
#7075 = DIRECTION('center_axis',(0.,1.,0.)) ;
#7076 = DIRECTION('ref_axis',(0.427975386405345,0.,0.903790389764793)) ;
#7077 = DIRECTION('center_axis',(0.,1.,0.)) ;
#7078 = DIRECTION('ref_axis',(-0.450036391082836,0.,0.893010216459552)) ;
#7079 = DIRECTION('',(0.,1.,0.)) ;
#7080 = DIRECTION('center_axis',(0.,1.,0.)) ;
#7081 = DIRECTION('ref_axis',(-0.450036391082836,0.,0.893010216459552)) ;
#7082 = DIRECTION('center_axis',(0.,1.,0.)) ;
#7083 = DIRECTION('ref_axis',(-0.9998388850409,0.,0.0179500406732147)) ;
#7084 = DIRECTION('',(0.,1.,0.)) ;
#7085 = DIRECTION('center_axis',(0.,1.,0.)) ;
#7086 = DIRECTION('ref_axis',(-0.9998388850409,0.,0.0179500406732147)) ;
#7087 = DIRECTION('center_axis',(-1.,0.,0.)) ;
#7088 = DIRECTION('ref_axis',(0.,0.,1.)) ;
#7089 = DIRECTION('',(0.,1.,0.)) ;
#7090 = DIRECTION('',(0.,0.,-1.)) ;
#7091 = DIRECTION('center_axis',(0.,1.,0.)) ;
#7092 = DIRECTION('ref_axis',(0.,0.,-1.)) ;
#7093 = DIRECTION('',(0.,1.,0.)) ;
#7094 = DIRECTION('center_axis',(0.,1.,0.)) ;
#7095 = DIRECTION('ref_axis',(0.,0.,-1.)) ;
#7096 = DIRECTION('center_axis',(0.,0.,-1.)) ;
#7097 = DIRECTION('ref_axis',(-1.,0.,0.)) ;
#7098 = DIRECTION('',(1.,0.,0.)) ;
#7099 = DIRECTION('',(0.,-1.,0.)) ;
#7100 = DIRECTION('',(1.,0.,0.)) ;
#7101 = DIRECTION('center_axis',(1.,0.,0.)) ;
#7102 = DIRECTION('ref_axis',(0.,0.,-1.)) ;
#7103 = DIRECTION('',(1.,0.,0.)) ;
#7104 = DIRECTION('center_axis',(-1.,0.,0.)) ;
#7105 = DIRECTION('ref_axis',(0.,0.,-1.)) ;
#7106 = DIRECTION('center_axis',(1.,0.,0.)) ;
#7107 = DIRECTION('ref_axis',(0.,0.,-1.)) ;
#7108 = DIRECTION('center_axis',(1.,0.,0.)) ;
#7109 = DIRECTION('ref_axis',(0.,0.,-1.)) ;
#7110 = DIRECTION('',(1.,0.,0.)) ;
#7111 = DIRECTION('center_axis',(1.,0.,0.)) ;
#7112 = DIRECTION('ref_axis',(0.,0.,-1.)) ;
#7113 = DIRECTION('',(0.,0.,-1.)) ;
#7114 = DIRECTION('',(0.,-1.,0.)) ;
#7115 = DIRECTION('',(0.,0.,1.)) ;
#7116 = DIRECTION('center_axis',(1.,0.,0.)) ;
#7117 = DIRECTION('ref_axis',(0.,0.,-1.)) ;
#7118 = DIRECTION('',(0.,-1.,0.)) ;
#7119 = DIRECTION('center_axis',(1.,0.,0.)) ;
#7120 = DIRECTION('ref_axis',(0.,0.00361481447269016,-0.999993466536821)) ;
#7121 = DIRECTION('center_axis',(0.,0.,1.)) ;
#7122 = DIRECTION('ref_axis',(0.,-1.,0.)) ;
#7123 = DIRECTION('',(0.,-1.,0.)) ;
#7124 = DIRECTION('',(1.,0.,0.)) ;
#7125 = DIRECTION('',(1.,0.,0.)) ;
#7126 = DIRECTION('center_axis',(0.,1.,0.)) ;
#7127 = DIRECTION('ref_axis',(0.,0.,1.)) ;
#7128 = DIRECTION('',(0.,0.,1.)) ;
#7129 = DIRECTION('',(1.,0.,0.)) ;
#7130 = DIRECTION('center_axis',(1.,0.,0.)) ;
#7131 = DIRECTION('ref_axis',(0.,0.,-1.)) ;
#7132 = DIRECTION('center_axis',(1.,0.,0.)) ;
#7133 = DIRECTION('ref_axis',(0.,0.,-1.)) ;
#7134 = DIRECTION('',(1.,0.,0.)) ;
#7135 = DIRECTION('center_axis',(0.,0.,1.)) ;
#7136 = DIRECTION('ref_axis',(0.,-1.,0.)) ;
#7137 = DIRECTION('',(-1.,0.,0.)) ;
#7138 = DIRECTION('',(0.,-1.,0.)) ;
#7139 = DIRECTION('center_axis',(1.,0.,0.)) ;
#7140 = DIRECTION('ref_axis',(0.,0.,-1.)) ;
#7141 = DIRECTION('center_axis',(-1.,0.,0.)) ;
#7142 = DIRECTION('ref_axis',(0.,0.00361481447269016,-0.999993466536821)) ;
#7143 = DIRECTION('',(0.,0.,1.)) ;
#7144 = DIRECTION('center_axis',(0.,1.,0.)) ;
#7145 = DIRECTION('ref_axis',(1.,0.,0.)) ;
#7146 = DIRECTION('',(-1.,0.,0.)) ;
#7147 = DIRECTION('center_axis',(0.,-1.,0.)) ;
#7148 = DIRECTION('ref_axis',(8.33188010975728E-16,0.,1.)) ;
#7149 = DIRECTION('',(-1.,0.,0.)) ;
#7150 = DIRECTION('center_axis',(0.,-1.,0.)) ;
#7151 = DIRECTION('ref_axis',(8.33188010975728E-16,0.,1.)) ;
#7152 = DIRECTION('center_axis',(0.,0.245126981107871,0.969490981460344)) ;
#7153 = DIRECTION('ref_axis',(0.,-0.969490981460344,0.245126981107871)) ;
#7154 = DIRECTION('',(1.,0.,0.)) ;
#7155 = DIRECTION('center_axis',(1.,0.,0.)) ;
#7156 = DIRECTION('ref_axis',(0.,0.00361481447269016,-0.999993466536821)) ;
#7157 = DIRECTION('center_axis',(0.,0.,-1.)) ;
#7158 = DIRECTION('ref_axis',(-1.,0.,0.)) ;
#7159 = DIRECTION('',(0.,1.,0.)) ;
#7160 = DIRECTION('center_axis',(0.,1.,0.)) ;
#7161 = DIRECTION('ref_axis',(8.33188010975728E-16,0.,1.)) ;
#7162 = DIRECTION('center_axis',(0.,0.,-1.)) ;
#7163 = DIRECTION('ref_axis',(-1.,0.,0.)) ;
#7164 = DIRECTION('',(0.,1.,0.)) ;
#7165 = DIRECTION('center_axis',(0.,1.,0.)) ;
#7166 = DIRECTION('ref_axis',(8.33188010975728E-16,0.,1.)) ;
#7167 = DIRECTION('axis',(0.,0.,1.)) ;
#7168 = DIRECTION('refdir',(1.,0.,0.)) ;
#7169 = DIRECTION('center_axis',(0.,0.,-1.)) ;
#7170 = DIRECTION('ref_axis',(0.707106781186546,-0.707106781186549,0.)) ;
#7171 = DIRECTION('',(0.,0.,1.)) ;
#7172 = DIRECTION('',(0.,0.,-1.)) ;
#7173 = DIRECTION('center_axis',(-1.,0.,0.)) ;
#7174 = DIRECTION('ref_axis',(0.,-0.813733471206731,0.581238193719102)) ;
#7175 = DIRECTION('center_axis',(1.,0.,0.)) ;
#7176 = DIRECTION('ref_axis',(0.,-0.813733471206731,0.581238193719102)) ;
#7177 = DIRECTION('center_axis',(0.,-0.940315265291054,-0.340304572200573)) ;
#7178 = DIRECTION('ref_axis',(0.707106781186547,-0.240631670671808,0.664903300540534)) ;
#7179 = DIRECTION('',(0.,0.940315265291054,0.340304572200573)) ;
#7180 = DIRECTION('',(0.,-0.940315265291054,-0.340304572200573)) ;
#7181 = DIRECTION('center_axis',(-1.,0.,0.)) ;
#7182 = DIRECTION('ref_axis',(0.,0.,1.)) ;
#7183 = DIRECTION('center_axis',(1.,0.,0.)) ;
#7184 = DIRECTION('ref_axis',(0.,0.554700196225229,-0.832050294337844)) ;
#7185 = DIRECTION('center_axis',(-1.,0.,0.)) ;
#7186 = DIRECTION('ref_axis',(0.,0.554700196225229,-0.832050294337844)) ;
#7187 = DIRECTION('center_axis',(0.,-0.561501418337265,-0.827475774391758)) ;
#7188 = DIRECTION('ref_axis',(0.707106781186551,-0.585113731339998,0.397041460552144)) ;
#7189 = DIRECTION('',(0.,0.561501418337265,0.827475774391758)) ;
#7190 = DIRECTION('',(0.,-0.561501418337265,-0.827475774391758)) ;
#7191 = DIRECTION('center_axis',(1.,0.,0.)) ;
#7192 = DIRECTION('ref_axis',(0.,0.,-1.)) ;
#7193 = DIRECTION('center_axis',(-1.,0.,0.)) ;
#7194 = DIRECTION('ref_axis',(0.,-0.86974260015344,-0.493505632671334)) ;
#7195 = DIRECTION('center_axis',(1.,0.,0.)) ;
#7196 = DIRECTION('ref_axis',(0.,-0.86974260015344,-0.493505632671334)) ;
#7197 = DIRECTION('center_axis',(0.,0.239567708183828,-0.970879659481827)) ;
#7198 = DIRECTION('ref_axis',(0.707106781186544,-0.68651559093569,-0.169399951010105)) ;
#7199 = DIRECTION('',(0.,0.239567708183828,-0.970879659481827)) ;
#7200 = DIRECTION('',(0.,-0.239567708183828,0.970879659481827)) ;
#7201 = DIRECTION('center_axis',(1.,0.,0.)) ;
#7202 = DIRECTION('ref_axis',(0.,0.,-1.)) ;
#7203 = DIRECTION('center_axis',(-1.,0.,0.)) ;
#7204 = DIRECTION('ref_axis',(0.,-0.570395809495344,0.821369965673296)) ;
#7205 = DIRECTION('center_axis',(1.,0.,0.)) ;
#7206 = DIRECTION('ref_axis',(0.,-0.570395809495344,0.821369965673296)) ;
#7207 = DIRECTION('center_axis',(0.,0.707106781186548,-0.707106781186548)) ;
#7208 = DIRECTION('ref_axis',(0.707106781186552,-0.499999999999989,-0.500000000000005)) ;
#7209 = DIRECTION('',(0.,0.707106781186548,-0.707106781186548)) ;
#7210 = DIRECTION('',(0.,-0.707106781186548,0.707106781186548)) ;
#7211 = DIRECTION('center_axis',(-1.,0.,0.)) ;
#7212 = DIRECTION('ref_axis',(0.,0.707106781186552,-0.707106781186543)) ;
#7213 = DIRECTION('center_axis',(1.,0.,0.)) ;
#7214 = DIRECTION('ref_axis',(0.,0.707106781186551,-0.707106781186544)) ;
#7215 = DIRECTION('center_axis',(-1.,0.,0.)) ;
#7216 = DIRECTION('ref_axis',(0.,0.707106781186551,-0.707106781186544)) ;
#7217 = DIRECTION('center_axis',(0.,0.,1.)) ;
#7218 = DIRECTION('ref_axis',(0.707106781186548,0.707106781186548,0.)) ;
#7219 = DIRECTION('',(0.,0.,-1.)) ;
#7220 = DIRECTION('',(0.,0.,1.)) ;
#7221 = DIRECTION('center_axis',(0.,0.0518000861243686,0.998657474351195)) ;
#7222 = DIRECTION('ref_axis',(0.707106781186548,0.70615747219636,-0.0366281921646092)) ;
#7223 = DIRECTION('',(0.,0.0518000861243686,0.998657474351195)) ;
#7224 = DIRECTION('',(0.,-0.0518000861243686,-0.998657474351195)) ;
#7225 = DIRECTION('center_axis',(0.,0.060701587016572,0.998155958422164)) ;
#7226 = DIRECTION('ref_axis',(0.,0.998155958422164,-0.060701587016572)) ;
#7227 = DIRECTION('center_axis',(-1.,0.,0.)) ;
#7228 = DIRECTION('ref_axis',(0.,0.,1.)) ;
#7229 = DIRECTION('center_axis',(1.,0.,0.)) ;
#7230 = DIRECTION('ref_axis',(0.,-0.860291533634174,-0.509802390301733)) ;
#7231 = DIRECTION('center_axis',(-1.,0.,0.)) ;
#7232 = DIRECTION('ref_axis',(0.,-0.860291533634174,-0.509802390301733)) ;
#7233 = DIRECTION('center_axis',(1.,0.,0.)) ;
#7234 = DIRECTION('ref_axis',(0.,0.,-1.)) ;
#7235 = DIRECTION('center_axis',(1.,0.,0.)) ;
#7236 = DIRECTION('ref_axis',(0.,0.933269707299496,0.359176354228828)) ;
#7237 = DIRECTION('center_axis',(-1.,0.,0.)) ;
#7238 = DIRECTION('ref_axis',(0.,0.933269707299496,0.359176354228828)) ;
#7239 = DIRECTION('center_axis',(1.,0.,0.)) ;
#7240 = DIRECTION('ref_axis',(0.,0.,-1.)) ;
#7241 = DIRECTION('center_axis',(-1.,0.,0.)) ;
#7242 = DIRECTION('ref_axis',(0.,0.867757267880784,0.49698825342263)) ;
#7243 = DIRECTION('center_axis',(1.,0.,0.)) ;
#7244 = DIRECTION('ref_axis',(0.,0.867757267880784,0.49698825342263)) ;
#7245 = DIRECTION('center_axis',(-1.,0.,0.)) ;
#7246 = DIRECTION('ref_axis',(0.,0.,1.)) ;
#7247 = DIRECTION('center_axis',(1.,0.,0.)) ;
#7248 = DIRECTION('ref_axis',(0.,-0.923683059121558,-0.383157417117091)) ;
#7249 = DIRECTION('center_axis',(0.,-0.706713794874047,0.707499549211675)) ;
#7250 = DIRECTION('ref_axis',(1.,0.,0.)) ;
#7251 = DIRECTION('center_axis',(-1.,0.,0.)) ;
#7252 = DIRECTION('ref_axis',(0.,-0.923683059121558,-0.383157417117091)) ;
#7253 = DIRECTION('center_axis',(0.,0.,1.)) ;
#7254 = DIRECTION('ref_axis',(0.70710678118654,0.707106781186555,0.)) ;
#7255 = DIRECTION('',(0.,0.,-1.)) ;
#7256 = DIRECTION('',(0.,0.,1.)) ;
#7257 = DIRECTION('center_axis',(0.,-0.707106781186548,0.707106781186548)) ;
#7258 = DIRECTION('ref_axis',(0.707106781186552,0.499999999999989,0.500000000000005)) ;
#7259 = DIRECTION('',(0.,-0.707106781186548,0.707106781186548)) ;
#7260 = DIRECTION('',(0.,0.707106781186548,-0.707106781186548)) ;
#7261 = DIRECTION('center_axis',(0.,0.0695982628490372,0.997575100836221)) ;
#7262 = DIRECTION('ref_axis',(0.707106781186555,0.705392118544138,-0.049213403619365)) ;
#7263 = DIRECTION('',(0.,0.0695982628490372,0.997575100836221)) ;
#7264 = DIRECTION('',(0.,-0.0695982628490372,-0.997575100836221)) ;
#7265 = DIRECTION('center_axis',(1.,0.,0.)) ;
#7266 = DIRECTION('ref_axis',(0.,4.0179797404504E-5,0.999999999192792)) ;
#7267 = DIRECTION('center_axis',(-1.,0.,0.)) ;
#7268 = DIRECTION('ref_axis',(0.,0.,1.)) ;
#7269 = DIRECTION('center_axis',(1.,0.,0.)) ;
#7270 = DIRECTION('ref_axis',(0.,0.,1.)) ;
#7271 = DIRECTION('center_axis',(1.,0.,0.)) ;
#7272 = DIRECTION('ref_axis',(0.,0.,-1.)) ;
#7273 = DIRECTION('center_axis',(1.,0.,0.)) ;
#7274 = DIRECTION('ref_axis',(0.,-0.649652327582147,-0.760231447170596)) ;
#7275 = DIRECTION('center_axis',(-1.,0.,0.)) ;
#7276 = DIRECTION('ref_axis',(0.,-0.649652327582147,-0.760231447170596)) ;
#7277 = DIRECTION('center_axis',(0.,0.,-1.)) ;
#7278 = DIRECTION('ref_axis',(0.707106781186548,-0.707106781186548,0.)) ;
#7279 = DIRECTION('',(0.,0.,1.)) ;
#7280 = DIRECTION('',(0.,0.,-1.)) ;
#7281 = DIRECTION('center_axis',(-1.,0.,0.)) ;
#7282 = DIRECTION('ref_axis',(0.,0.,1.)) ;
#7283 = DIRECTION('center_axis',(-1.,0.,0.)) ;
#7284 = DIRECTION('ref_axis',(0.,0.929577903322658,0.368625720283123)) ;
#7285 = DIRECTION('center_axis',(0.,0.0262932027111255,0.999654273982356)) ;
#7286 = DIRECTION('ref_axis',(0.,-0.999654273982356,0.0262932027111255)) ;
#7287 = DIRECTION('center_axis',(1.,0.,0.)) ;
#7288 = DIRECTION('ref_axis',(0.,0.929577903322658,0.368625720283123)) ;
#7289 = DIRECTION('center_axis',(0.,-0.0257899447975391,-0.999667384056987)) ;
#7290 = DIRECTION('ref_axis',(0.707106781186539,-0.706871586197721,0.0182362448527659)) ;
#7291 = DIRECTION('',(0.,0.0257899447975391,0.999667384056987)) ;
#7292 = DIRECTION('',(0.,-0.0257899447975391,-0.999667384056987)) ;
#7293 = DIRECTION('center_axis',(-1.,0.,0.)) ;
#7294 = DIRECTION('ref_axis',(0.,0.,1.)) ;
#7295 = DIRECTION('center_axis',(-1.,0.,0.)) ;
#7296 = DIRECTION('ref_axis',(0.,0.906183139995266,0.422885465331122)) ;
#7297 = DIRECTION('center_axis',(1.,0.,0.)) ;
#7298 = DIRECTION('ref_axis',(0.,0.906183139995266,0.422885465331122)) ;
#7299 = DIRECTION('center_axis',(0.,0.863187603129405,-0.504883315037953)) ;
#7300 = DIRECTION('ref_axis',(0.707106781186553,-0.357006415771267,-0.610365807608966)) ;
#7301 = DIRECTION('',(0.,0.863187603129405,-0.504883315037953)) ;
#7302 = DIRECTION('',(0.,-0.863187603129405,0.504883315037953)) ;
#7303 = DIRECTION('center_axis',(-1.,0.,0.)) ;
#7304 = DIRECTION('ref_axis',(0.,0.,1.)) ;
#7305 = DIRECTION('center_axis',(1.,0.,0.)) ;
#7306 = DIRECTION('ref_axis',(0.,-0.0970999642854239,0.995274633925616)) ;
#7307 = DIRECTION('center_axis',(-1.,0.,0.)) ;
#7308 = DIRECTION('ref_axis',(0.,-0.0970999642854239,0.995274633925616)) ;
#7309 = DIRECTION('center_axis',(0.,0.940190624657783,0.340648777049922)) ;
#7310 = DIRECTION('ref_axis',(0.70710678118655,0.240875060254906,-0.664815166303532)) ;
#7311 = DIRECTION('',(0.,0.940190624657783,0.340648777049922)) ;
#7312 = DIRECTION('',(0.,-0.940190624657783,-0.340648777049922)) ;
#7313 = DIRECTION('center_axis',(1.,0.,0.)) ;
#7314 = DIRECTION('ref_axis',(0.,0.,-1.)) ;
#7315 = DIRECTION('center_axis',(1.,0.,0.)) ;
#7316 = DIRECTION('ref_axis',(0.,-0.624695047554424,-0.780868809443031)) ;
#7317 = DIRECTION('center_axis',(-1.,0.,0.)) ;
#7318 = DIRECTION('ref_axis',(0.,-0.624695047554424,-0.780868809443031)) ;
#7319 = DIRECTION('center_axis',(1.,0.,0.)) ;
#7320 = DIRECTION('ref_axis',(0.,-0.987974784374397,-0.154615088010078)) ;
#7321 = DIRECTION('',(1.,0.,0.)) ;
#7322 = DIRECTION('center_axis',(-1.,0.,0.)) ;
#7323 = DIRECTION('ref_axis',(0.,-0.624695047554424,-0.780868809443031)) ;
#7324 = DIRECTION('',(1.,0.,0.)) ;
#7325 = DIRECTION('center_axis',(0.,-1.,0.)) ;
#7326 = DIRECTION('ref_axis',(0.,0.,-1.)) ;
#7327 = DIRECTION('',(1.,0.,0.)) ;
#7328 = DIRECTION('',(0.,0.,1.)) ;
#7329 = DIRECTION('center_axis',(1.,0.,0.)) ;
#7330 = DIRECTION('ref_axis',(0.,-0.244681224382906,0.969603577981477)) ;
#7331 = DIRECTION('',(1.,0.,0.)) ;
#7332 = DIRECTION('center_axis',(-1.,0.,0.)) ;
#7333 = DIRECTION('ref_axis',(0.,-0.813733471206731,0.581238193719102)) ;
#7334 = DIRECTION('center_axis',(0.,-0.340304572200573,0.940315265291054)) ;
#7335 = DIRECTION('ref_axis',(0.,-0.940315265291054,-0.340304572200573)) ;
#7336 = DIRECTION('',(1.,0.,0.)) ;
#7337 = DIRECTION('',(0.,0.940315265291054,0.340304572200573)) ;
#7338 = DIRECTION('center_axis',(1.,0.,0.)) ;
#7339 = DIRECTION('ref_axis',(0.,0.361292570457734,-0.932452507386861)) ;
#7340 = DIRECTION('',(1.,0.,0.)) ;
#7341 = DIRECTION('center_axis',(1.,0.,0.)) ;
#7342 = DIRECTION('ref_axis',(0.,0.554700196225229,-0.832050294337844)) ;
#7343 = DIRECTION('center_axis',(0.,-0.827475774391758,0.561501418337265)) ;
#7344 = DIRECTION('ref_axis',(0.,-0.561501418337265,-0.827475774391758)) ;
#7345 = DIRECTION('',(1.,0.,0.)) ;
#7346 = DIRECTION('',(0.,0.561501418337265,0.827475774391758)) ;
#7347 = DIRECTION('center_axis',(1.,0.,0.)) ;
#7348 = DIRECTION('ref_axis',(0.,-0.0509372265161325,0.998701856889655)) ;
#7349 = DIRECTION('',(1.,0.,0.)) ;
#7350 = DIRECTION('center_axis',(-1.,0.,0.)) ;
#7351 = DIRECTION('ref_axis',(0.,-0.570395809495344,0.821369965673296)) ;
#7352 = DIRECTION('center_axis',(1.,0.,0.)) ;
#7353 = DIRECTION('ref_axis',(0.,-0.0803728928848199,-0.996764865998659)) ;
#7354 = DIRECTION('',(1.,0.,0.)) ;
#7355 = DIRECTION('center_axis',(1.,0.,0.)) ;
#7356 = DIRECTION('ref_axis',(0.,0.707106781186551,-0.707106781186544)) ;
#7357 = DIRECTION('center_axis',(0.,-1.,0.)) ;
#7358 = DIRECTION('ref_axis',(0.,0.,-1.)) ;
#7359 = DIRECTION('',(1.,0.,0.)) ;
#7360 = DIRECTION('',(0.,0.,1.)) ;
#7361 = DIRECTION('center_axis',(1.,0.,0.)) ;
#7362 = DIRECTION('ref_axis',(0.,0.999964987220335,0.0083680543398295)) ;
#7363 = DIRECTION('',(1.,0.,0.)) ;
#7364 = DIRECTION('center_axis',(-1.,0.,0.)) ;
#7365 = DIRECTION('ref_axis',(0.,0.,1.)) ;
#7366 = DIRECTION('center_axis',(0.,1.,0.)) ;
#7367 = DIRECTION('ref_axis',(0.,0.,1.)) ;
#7368 = DIRECTION('',(1.,0.,0.)) ;
#7369 = DIRECTION('',(0.,0.,-1.)) ;
#7370 = DIRECTION('center_axis',(1.,0.,0.)) ;
#7371 = DIRECTION('ref_axis',(0.,-0.998538306838623,-0.0540485871772473)) ;
#7372 = DIRECTION('',(1.,0.,0.)) ;
#7373 = DIRECTION('center_axis',(1.,0.,0.)) ;
#7374 = DIRECTION('ref_axis',(0.,-0.860291533634174,-0.509802390301733)) ;
#7375 = DIRECTION('center_axis',(1.,0.,0.)) ;
#7376 = DIRECTION('ref_axis',(0.,0.999980636834705,0.00622301821128131)) ;
#7377 = DIRECTION('',(1.,0.,0.)) ;
#7378 = DIRECTION('center_axis',(-1.,0.,0.)) ;
#7379 = DIRECTION('ref_axis',(0.,0.867757267880784,0.49698825342263)) ;
#7380 = DIRECTION('center_axis',(0.,1.,0.)) ;
#7381 = DIRECTION('ref_axis',(0.,0.,1.)) ;
#7382 = DIRECTION('',(1.,0.,0.)) ;
#7383 = DIRECTION('',(0.,0.,-1.)) ;
#7384 = DIRECTION('center_axis',(1.,0.,0.)) ;
#7385 = DIRECTION('ref_axis',(0.,-0.999998748960749,-0.00158179547895617)) ;
#7386 = DIRECTION('',(1.,0.,0.)) ;
#7387 = DIRECTION('center_axis',(1.,0.,0.)) ;
#7388 = DIRECTION('ref_axis',(0.,-0.923683059121558,-0.383157417117091)) ;
#7389 = DIRECTION('center_axis',(1.,0.,0.)) ;
#7390 = DIRECTION('ref_axis',(0.,0.,-1.)) ;
#7391 = DIRECTION('',(0.,0.,1.)) ;
#7392 = DIRECTION('center_axis',(1.,0.,0.)) ;
#7393 = DIRECTION('ref_axis',(0.,0.,-1.)) ;
#7394 = DIRECTION('',(0.,0.,-1.)) ;
#7395 = DIRECTION('center_axis',(1.,0.,0.)) ;
#7396 = DIRECTION('ref_axis',(0.,3.41514000732436E-15,1.)) ;
#7397 = DIRECTION('center_axis',(-1.,0.,0.)) ;
#7398 = DIRECTION('ref_axis',(0.,0.,-1.)) ;
#7399 = DIRECTION('center_axis',(1.,0.,0.)) ;
#7400 = DIRECTION('ref_axis',(0.,0.,-1.)) ;
#7401 = DIRECTION('center_axis',(1.,0.,0.)) ;
#7402 = DIRECTION('ref_axis',(0.,-0.624695047554424,-0.780868809443031)) ;
#7403 = DIRECTION('center_axis',(0.,0.940190624657783,0.340648777049922)) ;
#7404 = DIRECTION('ref_axis',(-0.707106781186527,0.240875060254903,-0.664815166303557)) ;
#7405 = DIRECTION('',(0.,0.940190624657783,0.340648777049922)) ;
#7406 = DIRECTION('',(0.,-0.940190624657783,-0.340648777049922)) ;
#7407 = DIRECTION('center_axis',(1.,0.,0.)) ;
#7408 = DIRECTION('ref_axis',(0.,-0.0927241376138027,0.995691837017748)) ;
#7409 = DIRECTION('center_axis',(-1.,0.,0.)) ;
#7410 = DIRECTION('ref_axis',(0.,-0.0970999642854239,0.995274633925616)) ;
#7411 = DIRECTION('center_axis',(1.,0.,0.)) ;
#7412 = DIRECTION('ref_axis',(0.,-0.0970999642854239,0.995274633925616)) ;
#7413 = DIRECTION('center_axis',(0.,0.863187603129405,-0.504883315037953)) ;
#7414 = DIRECTION('ref_axis',(-0.707106781186538,-0.357006415771298,-0.610365807608966)) ;
#7415 = DIRECTION('',(0.,0.863187603129405,-0.504883315037953)) ;
#7416 = DIRECTION('',(0.,-0.863187603129405,0.504883315037953)) ;
#7417 = DIRECTION('center_axis',(1.,0.,0.)) ;
#7418 = DIRECTION('ref_axis',(0.,0.,-1.)) ;
#7419 = DIRECTION('center_axis',(-1.,0.,0.)) ;
#7420 = DIRECTION('ref_axis',(0.,0.906183139995266,0.422885465331122)) ;
#7421 = DIRECTION('center_axis',(1.,0.,0.)) ;
#7422 = DIRECTION('ref_axis',(0.,0.906183139995266,0.422885465331122)) ;
#7423 = DIRECTION('center_axis',(0.,0.,-1.)) ;
#7424 = DIRECTION('ref_axis',(-0.707106781186532,-0.707106781186563,0.)) ;
#7425 = DIRECTION('',(0.,0.,-1.)) ;
#7426 = DIRECTION('center_axis',(1.,0.,0.)) ;
#7427 = DIRECTION('ref_axis',(0.,0.,-1.)) ;
#7428 = DIRECTION('center_axis',(-1.,0.,0.)) ;
#7429 = DIRECTION('ref_axis',(0.,0.929577903322658,0.368625720283123)) ;
#7430 = DIRECTION('center_axis',(0.,0.0262932027111255,0.999654273982356)) ;
#7431 = DIRECTION('ref_axis',(-1.,0.,0.)) ;
#7432 = DIRECTION('center_axis',(1.,0.,0.)) ;
#7433 = DIRECTION('ref_axis',(0.,0.929577903322658,0.368625720283123)) ;
#7434 = DIRECTION('center_axis',(0.,-0.0257899447975391,-0.999667384056987)) ;
#7435 = DIRECTION('ref_axis',(-0.707106781186531,-0.706871586197729,0.0182362448527662)) ;
#7436 = DIRECTION('',(0.,0.0257899447975391,0.999667384056987)) ;
#7437 = DIRECTION('',(0.,-0.0257899447975391,-0.999667384056987)) ;
#7438 = DIRECTION('center_axis',(1.,0.,0.)) ;
#7439 = DIRECTION('ref_axis',(0.,-4.0179797404504E-5,0.999999999192792)) ;
#7440 = DIRECTION('center_axis',(1.,0.,0.)) ;
#7441 = DIRECTION('ref_axis',(0.,0.,1.)) ;
#7442 = DIRECTION('center_axis',(1.,0.,0.)) ;
#7443 = DIRECTION('ref_axis',(0.,0.,-1.)) ;
#7444 = DIRECTION('center_axis',(1.,0.,0.)) ;
#7445 = DIRECTION('ref_axis',(0.,-0.649652327582147,-0.760231447170596)) ;
#7446 = DIRECTION('center_axis',(-1.,0.,0.)) ;
#7447 = DIRECTION('ref_axis',(0.,-0.649652327582147,-0.760231447170596)) ;
#7448 = DIRECTION('center_axis',(0.,0.0695982628490372,0.997575100836221)) ;
#7449 = DIRECTION('ref_axis',(-0.707106781186547,0.705392118544146,-0.0492134036193656)) ;
#7450 = DIRECTION('',(0.,0.0695982628490372,0.997575100836221)) ;
#7451 = DIRECTION('center_axis',(0.,-0.060701587016572,-0.998155958422164)) ;
#7452 = DIRECTION('ref_axis',(0.,-0.998155958422164,0.060701587016572)) ;
#7453 = DIRECTION('',(0.,-0.0695982628490372,-0.997575100836221)) ;
#7454 = DIRECTION('center_axis',(1.,0.,0.)) ;
#7455 = DIRECTION('ref_axis',(0.,0.,-1.)) ;
#7456 = DIRECTION('center_axis',(0.,-0.706713794874047,0.707499549211675)) ;
#7457 = DIRECTION('ref_axis',(0.,0.707499549211675,0.706713794874047)) ;
#7458 = DIRECTION('center_axis',(-1.,0.,0.)) ;
#7459 = DIRECTION('ref_axis',(0.,-0.923683059121558,-0.383157417117091)) ;
#7460 = DIRECTION('center_axis',(0.,-0.707106781186548,0.707106781186548)) ;
#7461 = DIRECTION('ref_axis',(-0.707106781186544,0.499999999999995,0.50000000000001)) ;
#7462 = DIRECTION('',(0.,-0.707106781186547,0.707106781186547)) ;
#7463 = DIRECTION('',(0.,0.707106781186548,-0.707106781186548)) ;
#7464 = DIRECTION('center_axis',(0.,0.,1.)) ;
#7465 = DIRECTION('ref_axis',(-0.707106781186548,0.707106781186548,0.)) ;
#7466 = DIRECTION('',(0.,0.,1.)) ;
#7467 = DIRECTION('center_axis',(1.,0.,0.)) ;
#7468 = DIRECTION('ref_axis',(0.,0.,-1.)) ;
#7469 = DIRECTION('center_axis',(1.,0.,0.)) ;
#7470 = DIRECTION('ref_axis',(0.,0.933269707299496,0.359176354228828)) ;
#7471 = DIRECTION('center_axis',(-1.,0.,0.)) ;
#7472 = DIRECTION('ref_axis',(0.,0.933269707299496,0.359176354228828)) ;
#7473 = DIRECTION('center_axis',(1.,0.,0.)) ;
#7474 = DIRECTION('ref_axis',(0.,0.,-1.)) ;
#7475 = DIRECTION('center_axis',(1.,0.,0.)) ;
#7476 = DIRECTION('ref_axis',(0.,0.867757267880784,0.49698825342263)) ;
#7477 = DIRECTION('center_axis',(0.,0.0518000861243686,0.998657474351195)) ;
#7478 = DIRECTION('ref_axis',(-0.70710678118654,0.706157472196368,-0.0366281921646096)) ;
#7479 = DIRECTION('',(0.,0.0518000861243686,0.998657474351195)) ;
#7480 = DIRECTION('',(0.,-0.0518000861243686,-0.998657474351195)) ;
#7481 = DIRECTION('center_axis',(1.,0.,0.)) ;
#7482 = DIRECTION('ref_axis',(0.,0.,-1.)) ;
#7483 = DIRECTION('center_axis',(-1.,0.,0.)) ;
#7484 = DIRECTION('ref_axis',(0.,-0.860291533634174,-0.509802390301733)) ;
#7485 = DIRECTION('center_axis',(0.,0.,1.)) ;
#7486 = DIRECTION('ref_axis',(-0.707106781186532,0.707106781186563,0.)) ;
#7487 = DIRECTION('',(0.,0.,1.)) ;
#7488 = DIRECTION('center_axis',(0.,0.707106781186548,-0.707106781186548)) ;
#7489 = DIRECTION('ref_axis',(-0.707106781186544,-0.499999999999995,-0.50000000000001)) ;
#7490 = DIRECTION('',(0.,0.707106781186548,-0.707106781186548)) ;
#7491 = DIRECTION('',(0.,-0.707106781186548,0.707106781186548)) ;
#7492 = DIRECTION('center_axis',(1.,0.,0.)) ;
#7493 = DIRECTION('ref_axis',(0.,0.,-1.)) ;
#7494 = DIRECTION('center_axis',(-1.,0.,0.)) ;
#7495 = DIRECTION('ref_axis',(0.,0.707106781186551,-0.707106781186544)) ;
#7496 = DIRECTION('center_axis',(0.,0.239567708183828,-0.970879659481827)) ;
#7497 = DIRECTION('ref_axis',(-0.707106781186536,-0.686515590935697,-0.169399951010107)) ;
#7498 = DIRECTION('',(0.,0.239567708183828,-0.970879659481827)) ;
#7499 = DIRECTION('',(0.,-0.239567708183828,0.970879659481827)) ;
#7500 = DIRECTION('center_axis',(1.,0.,0.)) ;
#7501 = DIRECTION('ref_axis',(0.,0.,-1.)) ;
#7502 = DIRECTION('center_axis',(-1.,0.,0.)) ;
#7503 = DIRECTION('ref_axis',(0.,-0.86974260015344,-0.493505632671334)) ;
#7504 = DIRECTION('center_axis',(1.,0.,0.)) ;
#7505 = DIRECTION('ref_axis',(0.,-0.86974260015344,-0.493505632671334)) ;
#7506 = DIRECTION('center_axis',(1.,0.,0.)) ;
#7507 = DIRECTION('ref_axis',(0.,0.,-1.)) ;
#7508 = DIRECTION('center_axis',(1.,0.,0.)) ;
#7509 = DIRECTION('ref_axis',(0.,-0.570395809495344,0.821369965673296)) ;
#7510 = DIRECTION('center_axis',(0.,-0.561501418337265,-0.827475774391758)) ;
#7511 = DIRECTION('ref_axis',(-0.707106781186543,-0.585113731340005,0.397041460552148)) ;
#7512 = DIRECTION('',(0.,-0.561501418337265,-0.827475774391758)) ;
#7513 = DIRECTION('center_axis',(1.,0.,0.)) ;
#7514 = DIRECTION('ref_axis',(0.,0.,-1.)) ;
#7515 = DIRECTION('center_axis',(-1.,0.,0.)) ;
#7516 = DIRECTION('ref_axis',(0.,0.554700196225229,-0.832050294337844)) ;
#7517 = DIRECTION('center_axis',(0.,-0.940315265291054,-0.340304572200573)) ;
#7518 = DIRECTION('ref_axis',(-0.707106781186555,-0.240631670671808,0.664903300540525)) ;
#7519 = DIRECTION('',(0.,-0.940315265291054,-0.340304572200573)) ;
#7520 = DIRECTION('center_axis',(1.,0.,0.)) ;
#7521 = DIRECTION('ref_axis',(0.,-0.813733471206731,0.581238193719102)) ;
#7522 = DIRECTION('center_axis',(0.,0.,-1.)) ;
#7523 = DIRECTION('ref_axis',(-0.707106781186542,-0.707106781186553,0.)) ;
#7524 = DIRECTION('',(0.,0.,-1.)) ;
#7525 = DIRECTION('center_axis',(0.,0.340648777049922,-0.940190624657783)) ;
#7526 = DIRECTION('ref_axis',(0.,0.940190624657783,0.340648777049922)) ;
#7527 = DIRECTION('',(1.,0.,0.)) ;
#7528 = DIRECTION('center_axis',(1.,0.,0.)) ;
#7529 = DIRECTION('ref_axis',(0.,0.151162933346644,0.98850886064923)) ;
#7530 = DIRECTION('',(1.,0.,0.)) ;
#7531 = DIRECTION('center_axis',(0.,-0.504883315037953,-0.863187603129405)) ;
#7532 = DIRECTION('ref_axis',(0.,0.863187603129405,-0.504883315037953)) ;
#7533 = DIRECTION('',(1.,0.,0.)) ;
#7534 = DIRECTION('center_axis',(1.,0.,0.)) ;
#7535 = DIRECTION('ref_axis',(0.,0.977033726269219,0.213084719612847)) ;
#7536 = DIRECTION('',(1.,0.,0.)) ;
#7537 = DIRECTION('center_axis',(0.,-0.970879659481827,-0.239567708183828)) ;
#7538 = DIRECTION('ref_axis',(0.,0.239567708183828,-0.970879659481827)) ;
#7539 = DIRECTION('',(1.,0.,0.)) ;
#7540 = DIRECTION('center_axis',(1.,0.,0.)) ;
#7541 = DIRECTION('ref_axis',(0.,-0.970609304322144,-0.240660712130757)) ;
#7542 = DIRECTION('',(1.,0.,0.)) ;
#7543 = DIRECTION('center_axis',(0.,-0.707106781186548,-0.707106781186548)) ;
#7544 = DIRECTION('ref_axis',(0.,0.707106781186548,-0.707106781186548)) ;
#7545 = DIRECTION('',(1.,0.,0.)) ;
#7546 = DIRECTION('center_axis',(1.,0.,0.)) ;
#7547 = DIRECTION('ref_axis',(0.,0.999654273982356,-0.0262932027111252)) ;
#7548 = DIRECTION('',(1.,0.,0.)) ;
#7549 = DIRECTION('center_axis',(0.,-0.999667384056987,0.0257899447975391)) ;
#7550 = DIRECTION('ref_axis',(0.,-0.0257899447975391,-0.999667384056987)) ;
#7551 = DIRECTION('',(1.,0.,0.)) ;
#7552 = DIRECTION('center_axis',(1.,0.,0.)) ;
#7553 = DIRECTION('ref_axis',(0.,-0.649652327582147,-0.760231447170596)) ;
#7554 = DIRECTION('',(1.,0.,0.)) ;
#7555 = DIRECTION('center_axis',(0.,0.997575100836221,-0.0695982628490372)) ;
#7556 = DIRECTION('ref_axis',(0.,0.0695982628490372,0.997575100836221)) ;
#7557 = DIRECTION('',(1.,0.,0.)) ;
#7558 = DIRECTION('center_axis',(0.,0.998657474351195,-0.0518000861243686)) ;
#7559 = DIRECTION('ref_axis',(0.,0.0518000861243686,0.998657474351195)) ;
#7560 = DIRECTION('',(1.,0.,0.)) ;
#7561 = DIRECTION('center_axis',(1.,0.,0.)) ;
#7562 = DIRECTION('ref_axis',(0.,0.998550602064355,-0.0538209542549495)) ;
#7563 = DIRECTION('',(1.,0.,0.)) ;
#7564 = DIRECTION('center_axis',(0.,0.707106781186548,0.707106781186548)) ;
#7565 = DIRECTION('ref_axis',(0.,-0.707106781186548,0.707106781186548)) ;
#7566 = DIRECTION('center_axis',(1.,0.,0.)) ;
#7567 = DIRECTION('ref_axis',(0.,0.,-1.)) ;
#7568 = DIRECTION('center_axis',(-1.,0.,0.)) ;
#7569 = DIRECTION('ref_axis',(0.,0.,-1.)) ;
#7570 = DIRECTION('',(0.,0.,-1.)) ;
#7571 = DIRECTION('center_axis',(-1.,0.,0.)) ;
#7572 = DIRECTION('ref_axis',(0.,3.41514000732436E-15,1.)) ;
#7573 = DIRECTION('',(0.,0.,1.)) ;
#7574 = DIRECTION('center_axis',(-1.,0.,0.)) ;
#7575 = DIRECTION('ref_axis',(0.,0.,-1.)) ;
#7576 = DIRECTION('center_axis',(0.,0.,-1.)) ;
#7577 = DIRECTION('ref_axis',(0.707106781186548,-0.707106781186548,0.)) ;
#7578 = DIRECTION('',(0.,0.,-1.)) ;
#7579 = DIRECTION('center_axis',(-1.,0.,0.)) ;
#7580 = DIRECTION('ref_axis',(0.,0.,1.)) ;
#7581 = DIRECTION('center_axis',(-1.,0.,0.)) ;
#7582 = DIRECTION('ref_axis',(0.,3.41514000732436E-15,1.)) ;
#7583 = DIRECTION('center_axis',(0.,0.,1.)) ;
#7584 = DIRECTION('ref_axis',(0.707106781186548,0.707106781186548,0.)) ;
#7585 = DIRECTION('',(0.,0.,1.)) ;
#7586 = DIRECTION('center_axis',(-1.,0.,0.)) ;
#7587 = DIRECTION('ref_axis',(0.,-2.36807622294973E-14,-1.)) ;
#7588 = DIRECTION('center_axis',(-1.,0.,0.)) ;
#7589 = DIRECTION('ref_axis',(0.,0.,-1.)) ;
#7590 = DIRECTION('center_axis',(1.,0.,0.)) ;
#7591 = DIRECTION('ref_axis',(0.,-0.99972751218626,-0.0233431227103509)) ;
#7592 = DIRECTION('',(1.,0.,0.)) ;
#7593 = DIRECTION('center_axis',(1.,0.,0.)) ;
#7594 = DIRECTION('ref_axis',(0.,0.,-1.)) ;
#7595 = DIRECTION('',(1.,0.,0.)) ;
#7596 = DIRECTION('center_axis',(0.,-1.,0.)) ;
#7597 = DIRECTION('ref_axis',(0.,0.,-1.)) ;
#7598 = DIRECTION('',(1.,0.,0.)) ;
#7599 = DIRECTION('',(0.,0.,1.)) ;
#7600 = DIRECTION('center_axis',(-1.,0.,0.)) ;
#7601 = DIRECTION('ref_axis',(0.,0.,1.)) ;
#7602 = DIRECTION('center_axis',(1.,0.,0.)) ;
#7603 = DIRECTION('ref_axis',(0.,3.41514000732436E-15,1.)) ;
#7604 = DIRECTION('center_axis',(-1.,0.,0.)) ;
#7605 = DIRECTION('ref_axis',(0.,-3.38296603278533E-15,-1.)) ;
#7606 = DIRECTION('center_axis',(0.,0.,1.)) ;
#7607 = DIRECTION('ref_axis',(-0.70710678118654,0.707106781186555,0.)) ;
#7608 = DIRECTION('',(0.,0.,-1.)) ;
#7609 = DIRECTION('center_axis',(0.,0.,-1.)) ;
#7610 = DIRECTION('ref_axis',(-0.70710678118654,-0.707106781186555,0.)) ;
#7611 = DIRECTION('center_axis',(1.,0.,0.)) ;
#7612 = DIRECTION('ref_axis',(0.,0.,-1.)) ;
#7613 = DIRECTION('',(-1.,0.,0.)) ;
#7614 = DIRECTION('center_axis',(0.,1.,0.)) ;
#7615 = DIRECTION('ref_axis',(0.,0.,1.)) ;
#7616 = DIRECTION('',(1.,0.,0.)) ;
#7617 = DIRECTION('center_axis',(1.,0.,0.)) ;
#7618 = DIRECTION('ref_axis',(0.,0.999727512186261,0.0233431227103372)) ;
#7619 = DIRECTION('axis',(0.,0.,1.)) ;
#7620 = DIRECTION('refdir',(1.,0.,0.)) ;
#7621 = DIRECTION('center_axis',(-1.,0.,0.)) ;
#7622 = DIRECTION('ref_axis',(0.,0.,1.)) ;
#7623 = DIRECTION('center_axis',(1.,0.,0.)) ;
#7624 = DIRECTION('ref_axis',(0.,0.,-1.)) ;
#7625 = DIRECTION('center_axis',(1.,0.,0.)) ;
#7626 = DIRECTION('ref_axis',(0.,1.,0.)) ;
#7627 = DIRECTION('center_axis',(1.,0.,0.)) ;
#7628 = DIRECTION('ref_axis',(0.,0.,-1.)) ;
#7629 = DIRECTION('',(-0.707106781186548,0.707106781186548,8.65956056235493E-17)) ;
#7630 = DIRECTION('center_axis',(1.,0.,0.)) ;
#7631 = DIRECTION('ref_axis',(0.,1.,0.)) ;
#7632 = DIRECTION('center_axis',(1.,0.,0.)) ;
#7633 = DIRECTION('ref_axis',(0.,0.,-1.)) ;
#7634 = DIRECTION('',(-1.,0.,0.)) ;
#7635 = DIRECTION('center_axis',(-1.,0.,0.)) ;
#7636 = DIRECTION('ref_axis',(0.,1.,0.)) ;
#7637 = DIRECTION('center_axis',(1.,0.,0.)) ;
#7638 = DIRECTION('ref_axis',(0.,0.,-1.)) ;
#7639 = DIRECTION('',(-0.707106781186548,-0.707106781186548,-8.65956056235493E-17)) ;
#7640 = DIRECTION('center_axis',(1.,0.,0.)) ;
#7641 = DIRECTION('ref_axis',(0.,0.,-1.)) ;
#7642 = DIRECTION('axis',(0.,0.,1.)) ;
#7643 = DIRECTION('refdir',(1.,0.,0.)) ;
#7644 = DIRECTION('center_axis',(-1.,0.,0.)) ;
#7645 = DIRECTION('ref_axis',(0.,0.,1.)) ;
#7646 = DIRECTION('center_axis',(1.,0.,0.)) ;
#7647 = DIRECTION('ref_axis',(0.,0.,-1.)) ;
#7648 = DIRECTION('center_axis',(1.,0.,0.)) ;
#7649 = DIRECTION('ref_axis',(0.,1.,0.)) ;
#7650 = DIRECTION('center_axis',(1.,0.,0.)) ;
#7651 = DIRECTION('ref_axis',(0.,0.,-1.)) ;
#7652 = DIRECTION('',(-1.,0.,0.)) ;
#7653 = DIRECTION('center_axis',(-1.,0.,0.)) ;
#7654 = DIRECTION('ref_axis',(0.,0.,1.)) ;
#7655 = DIRECTION('center_axis',(1.,0.,0.)) ;
#7656 = DIRECTION('ref_axis',(0.,0.,-1.)) ;
#7657 = DIRECTION('center_axis',(1.,0.,0.)) ;
#7658 = DIRECTION('ref_axis',(0.,1.,0.)) ;
#7659 = DIRECTION('center_axis',(1.,0.,0.)) ;
#7660 = DIRECTION('ref_axis',(0.,0.,-1.)) ;
#7661 = DIRECTION('',(-0.707106781186543,0.707106781186552,8.65956056235499E-17)) ;
#7662 = DIRECTION('center_axis',(1.,0.,0.)) ;
#7663 = DIRECTION('ref_axis',(0.,1.,0.)) ;
#7664 = DIRECTION('center_axis',(1.,0.,0.)) ;
#7665 = DIRECTION('ref_axis',(0.,0.,-1.)) ;
#7666 = DIRECTION('',(-1.,0.,0.)) ;
#7667 = DIRECTION('center_axis',(-1.,0.,0.)) ;
#7668 = DIRECTION('ref_axis',(0.,1.,0.)) ;
#7669 = DIRECTION('center_axis',(1.,0.,0.)) ;
#7670 = DIRECTION('ref_axis',(0.,0.,-1.)) ;
#7671 = DIRECTION('',(-0.707106781186543,-0.707106781186552,-8.65956056235499E-17)) ;
#7672 = DIRECTION('center_axis',(1.,0.,0.)) ;
#7673 = DIRECTION('ref_axis',(0.,0.,-1.)) ;
#7674 = DIRECTION('center_axis',(1.,0.,0.)) ;
#7675 = DIRECTION('ref_axis',(0.,0.,-1.)) ;
#7676 = DIRECTION('center_axis',(1.,0.,0.)) ;
#7677 = DIRECTION('ref_axis',(0.,1.,0.)) ;
#7678 = DIRECTION('center_axis',(1.,0.,0.)) ;
#7679 = DIRECTION('ref_axis',(0.,0.,-1.)) ;
#7680 = DIRECTION('',(-1.,0.,0.)) ;
#7681 = DIRECTION('center_axis',(1.,0.,0.)) ;
#7682 = DIRECTION('ref_axis',(0.,0.,-1.)) ;
#7683 = DIRECTION('axis',(0.,0.,1.)) ;
#7684 = DIRECTION('refdir',(1.,0.,0.)) ;
#7685 = DIRECTION('center_axis',(0.,0.,-1.)) ;
#7686 = DIRECTION('ref_axis',(-1.,0.,0.)) ;
#7687 = DIRECTION('center_axis',(0.,0.,1.)) ;
#7688 = DIRECTION('ref_axis',(1.,0.,0.)) ;
#7689 = DIRECTION('center_axis',(0.,0.,1.)) ;
#7690 = DIRECTION('ref_axis',(1.,0.,0.)) ;
#7691 = DIRECTION('center_axis',(0.,0.,1.)) ;
#7692 = DIRECTION('ref_axis',(1.,0.,0.)) ;
#7693 = DIRECTION('',(0.707106781186549,8.65956056235495E-17,-0.707106781186546)) ;
#7694 = DIRECTION('center_axis',(0.,0.,1.)) ;
#7695 = DIRECTION('ref_axis',(1.,0.,0.)) ;
#7696 = DIRECTION('center_axis',(0.,0.,1.)) ;
#7697 = DIRECTION('ref_axis',(1.,0.,0.)) ;
#7698 = DIRECTION('',(0.,0.,-1.)) ;
#7699 = DIRECTION('center_axis',(0.,0.,-1.)) ;
#7700 = DIRECTION('ref_axis',(1.,0.,0.)) ;
#7701 = DIRECTION('center_axis',(0.,0.,1.)) ;
#7702 = DIRECTION('ref_axis',(1.,0.,0.)) ;
#7703 = DIRECTION('',(-0.707106781186549,-8.65956056235495E-17,-0.707106781186546)) ;
#7704 = DIRECTION('center_axis',(0.,0.,1.)) ;
#7705 = DIRECTION('ref_axis',(1.,0.,0.)) ;
#7706 = DIRECTION('axis',(0.,0.,1.)) ;
#7707 = DIRECTION('refdir',(1.,0.,0.)) ;
#7708 = DIRECTION('center_axis',(0.,0.,1.)) ;
#7709 = DIRECTION('ref_axis',(1.,0.,0.)) ;
#7710 = DIRECTION('center_axis',(0.,0.,-1.)) ;
#7711 = DIRECTION('ref_axis',(1.,0.,0.)) ;
#7712 = DIRECTION('',(0.,0.,-1.)) ;
#7713 = DIRECTION('center_axis',(0.,0.,-1.)) ;
#7714 = DIRECTION('ref_axis',(1.,0.,0.)) ;
#7715 = DIRECTION('center_axis',(0.0336887316936593,0.999432373578559,0.)) ;
#7716 = DIRECTION('ref_axis',(-0.999432373578559,0.0336887316936593,0.)) ;
#7717 = DIRECTION('',(-0.999432373578559,0.0336887316936593,0.)) ;
#7718 = DIRECTION('',(0.,0.,1.)) ;
#7719 = DIRECTION('',(-0.999432373578559,0.0336887316936593,0.)) ;
#7720 = DIRECTION('',(0.,0.,1.)) ;
#7721 = DIRECTION('center_axis',(0.991098234868642,0.133132598713698,0.)) ;
#7722 = DIRECTION('ref_axis',(-0.133132598713698,0.991098234868642,0.)) ;
#7723 = DIRECTION('',(-0.133132598713698,0.991098234868642,0.)) ;
#7724 = DIRECTION('',(-0.133132598713698,0.991098234868642,0.)) ;
#7725 = DIRECTION('',(0.,0.,1.)) ;
#7726 = DIRECTION('center_axis',(1.,0.,0.)) ;
#7727 = DIRECTION('ref_axis',(0.,1.,0.)) ;
#7728 = DIRECTION('',(0.,1.,0.)) ;
#7729 = DIRECTION('',(0.,1.,0.)) ;
#7730 = DIRECTION('',(0.,0.,1.)) ;
#7731 = DIRECTION('center_axis',(0.447213595499958,-0.894427190999916,0.)) ;
#7732 = DIRECTION('ref_axis',(0.894427190999916,0.447213595499958,0.)) ;
#7733 = DIRECTION('',(0.894427190999916,0.447213595499958,0.)) ;
#7734 = DIRECTION('',(0.894427190999916,0.447213595499958,0.)) ;
#7735 = DIRECTION('',(0.,0.,1.)) ;
#7736 = DIRECTION('center_axis',(-0.00862036934418878,-0.999962843925898,
0.)) ;
#7737 = DIRECTION('ref_axis',(0.999962843925898,-0.00862036934418878,0.)) ;
#7738 = DIRECTION('',(0.999962843925898,-0.00862036934418878,0.)) ;
#7739 = DIRECTION('',(0.999962843925898,-0.00862036934418878,0.)) ;
#7740 = DIRECTION('',(0.,0.,1.)) ;
#7741 = DIRECTION('center_axis',(-0.151025398741513,-0.988529882671721,0.)) ;
#7742 = DIRECTION('ref_axis',(0.988529882671721,-0.151025398741513,0.)) ;
#7743 = DIRECTION('',(0.988529882671721,-0.151025398741513,0.)) ;
#7744 = DIRECTION('',(0.988529882671721,-0.151025398741513,0.)) ;
#7745 = DIRECTION('',(0.,0.,1.)) ;
#7746 = DIRECTION('center_axis',(-0.997785157856609,-0.0665190105237732,0.)) ;
#7747 = DIRECTION('ref_axis',(0.0665190105237732,-0.997785157856609,0.)) ;
#7748 = DIRECTION('',(0.0665190105237732,-0.997785157856609,0.)) ;
#7749 = DIRECTION('',(0.0665190105237732,-0.997785157856609,0.)) ;
#7750 = DIRECTION('',(0.,0.,1.)) ;
#7751 = DIRECTION('center_axis',(-1.,0.,0.)) ;
#7752 = DIRECTION('ref_axis',(0.,-1.,0.)) ;
#7753 = DIRECTION('',(0.,-1.,0.)) ;
#7754 = DIRECTION('',(0.,-1.,0.)) ;
#7755 = DIRECTION('',(0.,0.,1.)) ;
#7756 = DIRECTION('center_axis',(-0.996072640692687,0.0885397902837945,0.)) ;
#7757 = DIRECTION('ref_axis',(-0.0885397902837945,-0.996072640692687,0.)) ;
#7758 = DIRECTION('',(-0.0885397902837945,-0.996072640692687,0.)) ;
#7759 = DIRECTION('',(-0.0885397902837945,-0.996072640692687,0.)) ;
#7760 = DIRECTION('center_axis',(0.,0.,1.)) ;
#7761 = DIRECTION('ref_axis',(1.,0.,0.)) ;
#7762 = DIRECTION('center_axis',(0.,0.,1.)) ;
#7763 = DIRECTION('ref_axis',(1.,0.,0.)) ;
#7764 = DIRECTION('axis',(0.,0.,1.)) ;
#7765 = DIRECTION('refdir',(1.,0.,0.)) ;
#7766 = DIRECTION('center_axis',(1.,5.31464800688788E-17,4.4612515253641E-17)) ;
#7767 = DIRECTION('ref_axis',(0.,-0.642934102631547,0.76592149706962)) ;
#7768 = DIRECTION('',(9.24446373305873E-32,-0.642934102631548,0.765921497069619)) ;
#7769 = DIRECTION('',(6.93889390390722E-17,-0.76592149706962,-0.642934102631546)) ;
#7770 = DIRECTION('',(2.05699049867507E-32,-0.642934102631547,0.76592149706962)) ;
#7771 = DIRECTION('',(6.93889390390722E-17,-0.76592149706962,-0.642934102631546)) ;
#7772 = DIRECTION('center_axis',(0.5,-0.55679726583827,0.6633074737669)) ;
#7773 = DIRECTION('ref_axis',(-0.866025403784439,-0.321467051315774,0.38296074853481)) ;
#7774 = DIRECTION('',(-0.866025403784439,-0.321467051315774,0.38296074853481)) ;
#7775 = DIRECTION('',(-0.866025403784438,-0.321467051315774,0.38296074853481)) ;
#7776 = DIRECTION('',(6.93889390390722E-17,-0.76592149706962,-0.642934102631546)) ;
#7777 = DIRECTION('center_axis',(-0.5,-0.55679726583827,0.6633074737669)) ;
#7778 = DIRECTION('ref_axis',(-0.866025403784438,0.321467051315773,-0.38296074853481)) ;
#7779 = DIRECTION('',(-0.866025403784439,0.321467051315774,-0.38296074853481)) ;
#7780 = DIRECTION('',(-0.866025403784438,0.321467051315773,-0.38296074853481)) ;
#7781 = DIRECTION('',(6.93889390390722E-17,-0.76592149706962,-0.642934102631546)) ;
#7782 = DIRECTION('center_axis',(-1.,-1.82945775519164E-16,1.10016194411862E-16)) ;
#7783 = DIRECTION('ref_axis',(-2.01885846339482E-16,0.642934102631547,-0.76592149706962)) ;
#7784 = DIRECTION('',(-2.01885846339482E-16,0.642934102631548,-0.765921497069619)) ;
#7785 = DIRECTION('',(-2.01885846339482E-16,0.642934102631547,-0.76592149706962)) ;
#7786 = DIRECTION('',(-6.93889390390722E-17,0.76592149706962,0.642934102631546)) ;
#7787 = DIRECTION('center_axis',(0.5,0.55679726583827,-0.6633074737669)) ;
#7788 = DIRECTION('ref_axis',(0.866025403784439,-0.321467051315773,0.38296074853481)) ;
#7789 = DIRECTION('',(0.866025403784439,-0.321467051315774,0.38296074853481)) ;
#7790 = DIRECTION('',(6.93889390390722E-17,-0.76592149706962,-0.642934102631546)) ;
#7791 = DIRECTION('',(0.866025403784439,-0.321467051315773,0.38296074853481)) ;
#7792 = DIRECTION('center_axis',(-0.5,0.55679726583827,-0.6633074737669)) ;
#7793 = DIRECTION('ref_axis',(0.866025403784439,0.321467051315774,-0.38296074853481)) ;
#7794 = DIRECTION('',(0.866025403784439,0.321467051315774,-0.38296074853481)) ;
#7795 = DIRECTION('',(0.866025403784438,0.321467051315774,-0.38296074853481)) ;
#7796 = DIRECTION('center_axis',(6.93889390390722E-17,-0.76592149706962,-0.642934102631546)) ;
#7797 = DIRECTION('ref_axis',(-1.,0.,-1.07925429301481E-16)) ;
#7798 = DIRECTION('center_axis',(0.,0.765921497069619,0.642934102631548)) ;
#7799 = DIRECTION('ref_axis',(1.,0.,0.)) ;
#7800 = DIRECTION('center_axis',(0.,-0.765921497069619,-0.642934102631548)) ;
#7801 = DIRECTION('ref_axis',(1.,0.,0.)) ;
#7802 = DIRECTION('center_axis',(0.,-0.765921497069619,-0.642934102631548)) ;
#7803 = DIRECTION('ref_axis',(0.,0.642934102631547,-0.76592149706962)) ;
#7804 = DIRECTION('center_axis',(0.,-0.765921497069619,-0.642934102631548)) ;
#7805 = DIRECTION('ref_axis',(1.,0.,0.)) ;
#7806 = DIRECTION('',(8.65956056235489E-17,0.996211348261336,-0.08696522060762)) ;
#7807 = DIRECTION('center_axis',(0.,-0.765921497069619,-0.642934102631548)) ;
#7808 = DIRECTION('ref_axis',(0.,0.642934102631547,-0.76592149706962)) ;
#7809 = DIRECTION('center_axis',(0.,-0.765921497069619,-0.642934102631548)) ;
#7810 = DIRECTION('ref_axis',(1.,0.,0.)) ;
#7811 = DIRECTION('',(0.,0.765921497069619,0.642934102631548)) ;
#7812 = DIRECTION('center_axis',(0.,0.765921497069619,0.642934102631548)) ;
#7813 = DIRECTION('ref_axis',(0.,0.642934102631547,-0.76592149706962)) ;
#7814 = DIRECTION('center_axis',(0.,-0.765921497069619,-0.642934102631548)) ;
#7815 = DIRECTION('ref_axis',(1.,0.,0.)) ;
#7816 = DIRECTION('',(-8.43474823948308E-17,0.112472134319156,0.993654879222003)) ;
#7817 = DIRECTION('center_axis',(0.,-0.765921497069619,-0.642934102631548)) ;
#7818 = DIRECTION('ref_axis',(0.,0.642934102631547,-0.76592149706962)) ;
#7819 = DIRECTION('center_axis',(0.,-0.765921497069619,-0.642934102631548)) ;
#7820 = DIRECTION('ref_axis',(1.,0.,0.)) ;
#7821 = DIRECTION('',(0.,0.765921497069619,0.642934102631548)) ;
#7822 = DIRECTION('center_axis',(0.,0.765921497069619,0.642934102631548)) ;
#7823 = DIRECTION('ref_axis',(0.,0.642934102631547,-0.76592149706962)) ;
#7824 = DIRECTION('center_axis',(0.,-0.765921497069619,-0.642934102631548)) ;
#7825 = DIRECTION('ref_axis',(1.,0.,0.)) ;
#7826 = DIRECTION('',(-7.65030790430717E-17,0.196446457725814,0.980514553307079)) ;
#7827 = DIRECTION('center_axis',(0.,-0.765921497069619,-0.642934102631548)) ;
#7828 = DIRECTION('ref_axis',(-1.,0.,0.)) ;
#7829 = DIRECTION('axis',(0.,0.,1.)) ;
#7830 = DIRECTION('refdir',(1.,0.,0.)) ;
#7831 = DIRECTION('center_axis',(0.,-1.,0.)) ;
#7832 = DIRECTION('ref_axis',(1.,0.,0.)) ;
#7833 = DIRECTION('center_axis',(0.,-1.,0.)) ;
#7834 = DIRECTION('ref_axis',(1.,0.,0.)) ;
#7835 = DIRECTION('',(0.,1.,0.)) ;
#7836 = DIRECTION('center_axis',(0.,1.,0.)) ;
#7837 = DIRECTION('ref_axis',(1.,0.,0.)) ;
#7838 = DIRECTION('',(-0.707106781186547,0.707106781186548,-8.65956056235493E-17)) ;
#7839 = DIRECTION('center_axis',(1.,0.,0.)) ;
#7840 = DIRECTION('ref_axis',(0.,0.,-1.)) ;
#7841 = DIRECTION('center_axis',(1.,0.,0.)) ;
#7842 = DIRECTION('ref_axis',(0.,0.,-1.)) ;
#7843 = DIRECTION('center_axis',(0.,-1.,0.)) ;
#7844 = DIRECTION('ref_axis',(0.,0.,1.)) ;
#7845 = DIRECTION('center_axis',(-1.,0.,0.)) ;
#7846 = DIRECTION('ref_axis',(0.,-4.6427390085679E-16,-1.)) ;
#7847 = DIRECTION('center_axis',(-1.,0.,0.)) ;
#7848 = DIRECTION('ref_axis',(0.,-4.6427390085679E-16,-1.)) ;
#7849 = DIRECTION('center_axis',(1.,0.,0.)) ;
#7850 = DIRECTION('ref_axis',(0.,0.,-1.)) ;
#7851 = DIRECTION('center_axis',(0.,-1.,0.)) ;
#7852 = DIRECTION('ref_axis',(0.,0.,1.)) ;
#7853 = DIRECTION('center_axis',(-1.,0.,0.)) ;
#7854 = DIRECTION('ref_axis',(0.,0.,-1.)) ;
#7855 = DIRECTION('center_axis',(-1.,0.,0.)) ;
#7856 = DIRECTION('ref_axis',(0.,0.,-1.)) ;
#7857 = DIRECTION('center_axis',(0.,0.,1.)) ;
#7858 = DIRECTION('ref_axis',(1.,0.,0.)) ;
#7859 = DIRECTION('center_axis',(0.,0.,1.)) ;
#7860 = DIRECTION('ref_axis',(1.,0.,0.)) ;
#7861 = DIRECTION('',(0.,0.,-1.)) ;
#7862 = DIRECTION('center_axis',(0.,0.,-1.)) ;
#7863 = DIRECTION('ref_axis',(0.,1.,0.)) ;
#7864 = DIRECTION('center_axis',(0.,0.,-1.)) ;
#7865 = DIRECTION('ref_axis',(1.,0.,0.)) ;
#7866 = DIRECTION('',(-0.707106781186549,-8.65956056235495E-17,-0.707106781186546)) ;
#7867 = DIRECTION('center_axis',(1.,0.,0.)) ;
#7868 = DIRECTION('ref_axis',(0.,0.,-1.)) ;
#7869 = DIRECTION('center_axis',(1.,0.,0.)) ;
#7870 = DIRECTION('ref_axis',(0.,0.,-1.)) ;
#7871 = DIRECTION('center_axis',(0.,-1.,0.)) ;
#7872 = DIRECTION('ref_axis',(0.,0.,1.)) ;
#7873 = DIRECTION('center_axis',(1.,0.,0.)) ;
#7874 = DIRECTION('ref_axis',(0.,0.,-1.)) ;
#7875 = DIRECTION('center_axis',(0.,-1.,0.)) ;
#7876 = DIRECTION('ref_axis',(0.,0.,1.)) ;
#7877 = DIRECTION('axis',(0.,0.,1.)) ;
#7878 = DIRECTION('refdir',(1.,0.,0.)) ;
#7879 = DIRECTION('center_axis',(1.,0.,0.)) ;
#7880 = DIRECTION('ref_axis',(0.,1.,0.)) ;
#7881 = DIRECTION('center_axis',(1.,0.,0.)) ;
#7882 = DIRECTION('ref_axis',(0.,0.,-1.)) ;
#7883 = DIRECTION('',(-1.,0.,0.)) ;
#7884 = DIRECTION('center_axis',(1.,0.,0.)) ;
#7885 = DIRECTION('ref_axis',(0.,0.,-1.)) ;
#7886 = DIRECTION('center_axis',(-1.,0.,0.)) ;
#7887 = DIRECTION('ref_axis',(0.,0.,1.)) ;
#7888 = DIRECTION('center_axis',(1.,0.,0.)) ;
#7889 = DIRECTION('ref_axis',(0.,0.,-1.)) ;
#7890 = DIRECTION('center_axis',(1.,0.,0.)) ;
#7891 = DIRECTION('ref_axis',(0.,1.,0.)) ;
#7892 = DIRECTION('center_axis',(1.,0.,0.)) ;
#7893 = DIRECTION('ref_axis',(0.,0.,-1.)) ;
#7894 = DIRECTION('',(-1.,0.,0.)) ;
#7895 = DIRECTION('center_axis',(1.,0.,0.)) ;
#7896 = DIRECTION('ref_axis',(0.,0.,-1.)) ;
#7897 = DIRECTION('axis',(0.,0.,1.)) ;
#7898 = DIRECTION('refdir',(1.,0.,0.)) ;
#7899 = DIRECTION('center_axis',(1.,0.,0.)) ;
#7900 = DIRECTION('ref_axis',(0.,1.,0.)) ;
#7901 = DIRECTION('center_axis',(1.,0.,0.)) ;
#7902 = DIRECTION('ref_axis',(0.,0.,-1.)) ;
#7903 = DIRECTION('',(-1.,0.,0.)) ;
#7904 = DIRECTION('center_axis',(1.,0.,0.)) ;
#7905 = DIRECTION('ref_axis',(0.,0.,-1.)) ;
#7906 = DIRECTION('center_axis',(-1.,0.,0.)) ;
#7907 = DIRECTION('ref_axis',(0.,0.,1.)) ;
#7908 = DIRECTION('center_axis',(1.,0.,0.)) ;
#7909 = DIRECTION('ref_axis',(0.,0.,-1.)) ;
#7910 = DIRECTION('center_axis',(1.,0.,0.)) ;
#7911 = DIRECTION('ref_axis',(0.,1.,0.)) ;
#7912 = DIRECTION('center_axis',(1.,0.,0.)) ;
#7913 = DIRECTION('ref_axis',(0.,0.,-1.)) ;
#7914 = DIRECTION('',(-1.,0.,0.)) ;
#7915 = DIRECTION('center_axis',(1.,0.,0.)) ;
#7916 = DIRECTION('ref_axis',(0.,0.,-1.)) ;
#7917 = DIRECTION('axis',(0.,0.,1.)) ;
#7918 = DIRECTION('refdir',(1.,0.,0.)) ;
#7919 = DIRECTION('center_axis',(1.,0.,0.)) ;
#7920 = DIRECTION('ref_axis',(0.,1.,0.)) ;
#7921 = DIRECTION('center_axis',(1.,0.,0.)) ;
#7922 = DIRECTION('ref_axis',(0.,0.,-1.)) ;
#7923 = DIRECTION('',(-1.,0.,0.)) ;
#7924 = DIRECTION('center_axis',(1.,0.,0.)) ;
#7925 = DIRECTION('ref_axis',(0.,0.,-1.)) ;
#7926 = DIRECTION('center_axis',(-1.,0.,0.)) ;
#7927 = DIRECTION('ref_axis',(0.,0.,1.)) ;
#7928 = DIRECTION('center_axis',(1.,0.,0.)) ;
#7929 = DIRECTION('ref_axis',(0.,0.,-1.)) ;
#7930 = DIRECTION('center_axis',(1.,0.,0.)) ;
#7931 = DIRECTION('ref_axis',(0.,1.,0.)) ;
#7932 = DIRECTION('center_axis',(1.,0.,0.)) ;
#7933 = DIRECTION('ref_axis',(0.,0.,-1.)) ;
#7934 = DIRECTION('',(-1.,0.,0.)) ;
#7935 = DIRECTION('center_axis',(1.,0.,0.)) ;
#7936 = DIRECTION('ref_axis',(0.,0.,-1.)) ;
#7937 = DIRECTION('axis',(0.,0.,1.)) ;
#7938 = DIRECTION('refdir',(1.,0.,0.)) ;
#7939 = DIRECTION('center_axis',(1.,0.,0.)) ;
#7940 = DIRECTION('ref_axis',(0.,-1.,-6.96610525254997E-15)) ;
#7941 = DIRECTION('center_axis',(1.,0.,0.)) ;
#7942 = DIRECTION('ref_axis',(0.,-1.,-6.96610525254997E-15)) ;
#7943 = DIRECTION('',(1.,0.,0.)) ;
#7944 = DIRECTION('center_axis',(-1.,0.,0.)) ;
#7945 = DIRECTION('ref_axis',(0.,-1.,-6.96610525254997E-15)) ;
#7946 = DIRECTION('',(1.,0.,0.)) ;
#7947 = DIRECTION('center_axis',(0.,0.,1.)) ;
#7948 = DIRECTION('ref_axis',(0.,-1.,0.)) ;
#7949 = DIRECTION('',(0.,-1.,0.)) ;
#7950 = DIRECTION('',(0.,-1.,0.)) ;
#7951 = DIRECTION('',(1.,0.,0.)) ;
#7952 = DIRECTION('center_axis',(0.,0.72338954512527,-0.690440124850414)) ;
#7953 = DIRECTION('ref_axis',(0.,0.690440124850414,0.72338954512527)) ;
#7954 = DIRECTION('',(0.,0.690440124850414,0.72338954512527)) ;
#7955 = DIRECTION('',(0.,0.690440124850414,0.72338954512527)) ;
#7956 = DIRECTION('',(1.,0.,0.)) ;
#7957 = DIRECTION('center_axis',(1.,0.,0.)) ;
#7958 = DIRECTION('ref_axis',(0.,-0.885754641370607,-0.464153762551191)) ;
#7959 = DIRECTION('center_axis',(1.,0.,0.)) ;
#7960 = DIRECTION('ref_axis',(0.,-0.179181570317841,0.983816021854916)) ;
#7961 = DIRECTION('center_axis',(-1.,0.,0.)) ;
#7962 = DIRECTION('ref_axis',(0.,-0.179181570317841,0.983816021854916)) ;
#7963 = DIRECTION('',(1.,0.,0.)) ;
#7964 = DIRECTION('center_axis',(0.,0.708172501721611,0.70603945201763)) ;
#7965 = DIRECTION('ref_axis',(0.,-0.70603945201763,0.708172501721611)) ;
#7966 = DIRECTION('',(0.,-0.70603945201763,0.708172501721611)) ;
#7967 = DIRECTION('',(0.,-0.70603945201763,0.708172501721611)) ;
#7968 = DIRECTION('',(1.,0.,0.)) ;
#7969 = DIRECTION('center_axis',(1.,0.,0.)) ;
#7970 = DIRECTION('ref_axis',(0.,-0.911558251075126,-0.411170955804099)) ;
#7971 = DIRECTION('center_axis',(1.,0.,0.)) ;
#7972 = DIRECTION('ref_axis',(0.,-0.12333775780625,0.992364750230139)) ;
#7973 = DIRECTION('center_axis',(1.,0.,0.)) ;
#7974 = DIRECTION('ref_axis',(0.,-0.12333775780625,0.992364750230139)) ;
#7975 = DIRECTION('',(1.,0.,0.)) ;
#7976 = DIRECTION('center_axis',(1.,0.,0.)) ;
#7977 = DIRECTION('ref_axis',(0.,0.999988378789617,0.00482102537998268)) ;
#7978 = DIRECTION('center_axis',(1.,0.,0.)) ;
#7979 = DIRECTION('ref_axis',(0.,0.999988378789617,0.00482102537998268)) ;
#7980 = DIRECTION('center_axis',(1.,0.,0.)) ;
#7981 = DIRECTION('ref_axis',(0.,0.999988378789617,0.00482102537998268)) ;
#7982 = DIRECTION('',(1.,0.,0.)) ;
#7983 = DIRECTION('center_axis',(0.,1.,0.)) ;
#7984 = DIRECTION('ref_axis',(0.,0.,1.)) ;
#7985 = DIRECTION('',(0.,0.,1.)) ;
#7986 = DIRECTION('',(0.,0.,1.)) ;
#7987 = DIRECTION('center_axis',(1.,0.,0.)) ;
#7988 = DIRECTION('ref_axis',(0.,0.,-1.)) ;
#7989 = DIRECTION('center_axis',(1.,0.,0.)) ;
#7990 = DIRECTION('ref_axis',(0.,0.,-1.)) ;
#7991 = DIRECTION('axis',(0.,0.,1.)) ;
#7992 = DIRECTION('refdir',(1.,0.,0.)) ;
#7993 = DIRECTION('center_axis',(1.,0.,0.)) ;
#7994 = DIRECTION('ref_axis',(0.,0.,-1.)) ;
#7995 = DIRECTION('center_axis',(-1.,0.,0.)) ;
#7996 = DIRECTION('ref_axis',(0.,0.,-1.)) ;
#7997 = DIRECTION('',(-1.,0.,0.)) ;
#7998 = DIRECTION('center_axis',(-1.,0.,0.)) ;
#7999 = DIRECTION('ref_axis',(0.,0.,-1.)) ;
#8000 = DIRECTION('center_axis',(1.,0.,0.)) ;
#8001 = DIRECTION('ref_axis',(0.,-1.,-6.96610525254997E-15)) ;
#8002 = DIRECTION('center_axis',(1.,0.,0.)) ;
#8003 = DIRECTION('ref_axis',(0.,-1.,-6.96610525254997E-15)) ;
#8004 = DIRECTION('',(1.,0.,0.)) ;
#8005 = DIRECTION('center_axis',(-1.,0.,0.)) ;
#8006 = DIRECTION('ref_axis',(0.,-1.,-6.96610525254997E-15)) ;
#8007 = DIRECTION('',(1.,0.,0.)) ;
#8008 = DIRECTION('center_axis',(0.,0.,1.)) ;
#8009 = DIRECTION('ref_axis',(0.,-1.,0.)) ;
#8010 = DIRECTION('',(0.,-1.,0.)) ;
#8011 = DIRECTION('',(0.,-1.,0.)) ;
#8012 = DIRECTION('',(1.,0.,0.)) ;
#8013 = DIRECTION('center_axis',(1.,0.,0.)) ;
#8014 = DIRECTION('ref_axis',(0.,0.98957973940004,0.143985899896303)) ;
#8015 = DIRECTION('center_axis',(1.,0.,0.)) ;
#8016 = DIRECTION('ref_axis',(0.,0.98957973940004,0.143985899896303)) ;
#8017 = DIRECTION('center_axis',(1.,0.,0.)) ;
#8018 = DIRECTION('ref_axis',(0.,0.98957973940004,0.143985899896303)) ;
#8019 = DIRECTION('',(1.,0.,0.)) ;
#8020 = DIRECTION('center_axis',(1.,0.,0.)) ;
#8021 = DIRECTION('ref_axis',(0.,-0.143772557860476,-0.98961075762456)) ;
#8022 = DIRECTION('center_axis',(1.,0.,0.)) ;
#8023 = DIRECTION('ref_axis',(0.,-0.143772557860476,-0.98961075762456)) ;
#8024 = DIRECTION('center_axis',(1.,0.,0.)) ;
#8025 = DIRECTION('ref_axis',(0.,-0.143772557860476,-0.98961075762456)) ;
#8026 = DIRECTION('',(1.,0.,0.)) ;
#8027 = DIRECTION('center_axis',(0.,0.737154140200741,-0.675724628517347)) ;
#8028 = DIRECTION('ref_axis',(0.,0.675724628517347,0.737154140200741)) ;
#8029 = DIRECTION('',(0.,0.675724628517346,0.737154140200741)) ;
#8030 = DIRECTION('',(0.,0.675724628517346,0.737154140200741)) ;
#8031 = DIRECTION('',(1.,0.,0.)) ;
#8032 = DIRECTION('center_axis',(1.,0.,0.)) ;
#8033 = DIRECTION('ref_axis',(0.,-0.942609625269263,-0.333896831895331)) ;
#8034 = DIRECTION('center_axis',(1.,0.,0.)) ;
#8035 = DIRECTION('ref_axis',(0.,-0.942609625269263,-0.333896831895331)) ;
#8036 = DIRECTION('center_axis',(1.,0.,0.)) ;
#8037 = DIRECTION('ref_axis',(0.,-0.942609625269263,-0.333896831895331)) ;
#8038 = DIRECTION('',(1.,0.,0.)) ;
#8039 = DIRECTION('center_axis',(0.,-0.944836198498626,-0.327543215479523)) ;
#8040 = DIRECTION('ref_axis',(0.,0.327543215479523,-0.944836198498626)) ;
#8041 = DIRECTION('',(0.,0.327543215479523,-0.944836198498626)) ;
#8042 = DIRECTION('',(0.,0.327543215479523,-0.944836198498626)) ;
#8043 = DIRECTION('',(1.,0.,0.)) ;
#8044 = DIRECTION('center_axis',(1.,0.,0.)) ;
#8045 = DIRECTION('ref_axis',(0.,-0.122163634017166,0.992509973009702)) ;
#8046 = DIRECTION('center_axis',(1.,0.,0.)) ;
#8047 = DIRECTION('ref_axis',(0.,-0.122163634017166,0.992509973009702)) ;
#8048 = DIRECTION('center_axis',(1.,0.,0.)) ;
#8049 = DIRECTION('ref_axis',(0.,-0.122163634017166,0.992509973009702)) ;
#8050 = DIRECTION('',(1.,0.,0.)) ;
#8051 = DIRECTION('center_axis',(1.,0.,0.)) ;
#8052 = DIRECTION('ref_axis',(0.,0.999988378789617,0.00482102537998268)) ;
#8053 = DIRECTION('center_axis',(1.,0.,0.)) ;
#8054 = DIRECTION('ref_axis',(0.,0.999988378789617,0.00482102537998268)) ;
#8055 = DIRECTION('center_axis',(1.,0.,0.)) ;
#8056 = DIRECTION('ref_axis',(0.,0.999988378789617,0.00482102537998268)) ;
#8057 = DIRECTION('',(1.,0.,0.)) ;
#8058 = DIRECTION('center_axis',(0.,1.,0.)) ;
#8059 = DIRECTION('ref_axis',(0.,0.,1.)) ;
#8060 = DIRECTION('',(0.,0.,1.)) ;
#8061 = DIRECTION('',(0.,0.,1.)) ;
#8062 = DIRECTION('center_axis',(1.,0.,0.)) ;
#8063 = DIRECTION('ref_axis',(0.,0.,-1.)) ;
#8064 = DIRECTION('center_axis',(1.,0.,0.)) ;
#8065 = DIRECTION('ref_axis',(0.,0.,-1.)) ;
#8066 = DIRECTION('axis',(0.,0.,1.)) ;
#8067 = DIRECTION('refdir',(1.,0.,0.)) ;
#8068 = DIRECTION('center_axis',(1.,0.,0.)) ;
#8069 = DIRECTION('ref_axis',(0.,1.,0.)) ;
#8070 = DIRECTION('center_axis',(1.,0.,0.)) ;
#8071 = DIRECTION('ref_axis',(0.,0.,-1.)) ;
#8072 = DIRECTION('',(-1.,0.,0.)) ;
#8073 = DIRECTION('center_axis',(1.,0.,0.)) ;
#8074 = DIRECTION('ref_axis',(0.,0.,-1.)) ;
#8075 = DIRECTION('center_axis',(-1.,0.,0.)) ;
#8076 = DIRECTION('ref_axis',(0.,0.,1.)) ;
#8077 = DIRECTION('center_axis',(1.,0.,0.)) ;
#8078 = DIRECTION('ref_axis',(0.,0.,-1.)) ;
#8079 = DIRECTION('center_axis',(1.,0.,0.)) ;
#8080 = DIRECTION('ref_axis',(0.,1.,0.)) ;
#8081 = DIRECTION('center_axis',(1.,0.,0.)) ;
#8082 = DIRECTION('ref_axis',(0.,0.,-1.)) ;
#8083 = DIRECTION('',(-1.,0.,0.)) ;
#8084 = DIRECTION('center_axis',(1.,0.,0.)) ;
#8085 = DIRECTION('ref_axis',(0.,0.,-1.)) ;
#8086 = DIRECTION('',(0.,0.,1.)) ;
#8087 = DIRECTION('',(1.,0.,0.)) ;
#8088 = DIRECTION('',(0.,0.,1.)) ;
#8089 = DIRECTION('',(1.,0.,0.)) ;
#8090 = DIRECTION('',(0.,0.,1.)) ;
#8091 = DIRECTION('',(1.,0.,0.)) ;
#8092 = DIRECTION('',(0.,0.,1.)) ;
#8093 = DIRECTION('',(1.,0.,0.)) ;
#8094 = DIRECTION('',(0.,0.,1.)) ;
#8095 = DIRECTION('',(1.,0.,0.)) ;
#8096 = DIRECTION('',(0.,0.,1.)) ;
#8097 = DIRECTION('',(1.,0.,0.)) ;
#8098 = DIRECTION('',(0.,0.,1.)) ;
#8099 = DIRECTION('',(1.,0.,0.)) ;
#8100 = DIRECTION('',(0.,0.,1.)) ;
#8101 = DIRECTION('',(1.,0.,0.)) ;
#8102 = DIRECTION('',(0.,0.,1.)) ;
#8103 = DIRECTION('',(1.,0.,0.)) ;
#8104 = DIRECTION('',(0.,0.,1.)) ;
#8105 = DIRECTION('',(1.,0.,0.)) ;
#8106 = DIRECTION('',(0.,0.,1.)) ;
#8107 = DIRECTION('',(1.,0.,0.)) ;
#8108 = DIRECTION('',(0.,0.,1.)) ;
#8109 = DIRECTION('',(1.,0.,0.)) ;
#8110 = DIRECTION('',(0.,0.,1.)) ;
#8111 = DIRECTION('',(1.,0.,0.)) ;
#8112 = DIRECTION('',(0.,0.,1.)) ;
#8113 = DIRECTION('',(1.,0.,0.)) ;
#8114 = DIRECTION('',(0.,0.,1.)) ;
#8115 = DIRECTION('',(1.,0.,0.)) ;
#8116 = DIRECTION('',(0.,0.,1.)) ;
#8117 = DIRECTION('',(1.,0.,0.)) ;
#8118 = DIRECTION('',(0.,0.,1.)) ;
#8119 = DIRECTION('',(1.,0.,0.)) ;
#8120 = DIRECTION('',(0.,0.,1.)) ;
#8121 = DIRECTION('',(1.,0.,0.)) ;
#8122 = DIRECTION('',(0.,0.,1.)) ;
#8123 = DIRECTION('',(1.,0.,0.)) ;
#8124 = DIRECTION('',(0.,0.,1.)) ;
#8125 = DIRECTION('',(1.,0.,0.)) ;
#8126 = DIRECTION('',(1.22464679914735E-16,0.,-1.)) ;
#8127 = DIRECTION('',(-1.,0.,-1.22464679914735E-16)) ;
#8128 = CARTESIAN_POINT('',(0.,0.,0.)) ;
#8129 = CARTESIAN_POINT('',(0.,0.,0.)) ;
#8130 = CARTESIAN_POINT('Origin',(0.475,7.535,-29.)) ;
#8131 = CARTESIAN_POINT('',(-1.275,7.535,-28.55)) ;
#8132 = CARTESIAN_POINT('Origin',(0.475,7.535,-28.55)) ;
#8133 = CARTESIAN_POINT('',(-1.275,7.535,-20.)) ;
#8134 = CARTESIAN_POINT('',(-1.275,7.535,-29.)) ;
#8135 = CARTESIAN_POINT('Origin',(0.475,7.535,-20.)) ;
#8136 = CARTESIAN_POINT('Origin',(-30.,17.565,27.14)) ;
#8137 = CARTESIAN_POINT('',(-9.5,17.565,31.12)) ;
#8138 = CARTESIAN_POINT('Origin',(-9.5,17.565,27.14)) ;
#8139 = CARTESIAN_POINT('',(-6.35,17.565,31.12)) ;
#8140 = CARTESIAN_POINT('',(-30.,17.565,31.12)) ;
#8141 = CARTESIAN_POINT('Origin',(-6.35,17.565,27.14)) ;
#8142 = CARTESIAN_POINT('Origin',(-30.,17.565,27.14)) ;
#8143 = CARTESIAN_POINT('',(6.35,17.565,31.12)) ;
#8144 = CARTESIAN_POINT('Origin',(6.35,17.565,27.14)) ;
#8145 = CARTESIAN_POINT('',(9.5,17.565,31.12)) ;
#8146 = CARTESIAN_POINT('',(-30.,17.565,31.12)) ;
#8147 = CARTESIAN_POINT('Origin',(9.5,17.565,27.14)) ;
#8148 = CARTESIAN_POINT('Origin',(-6.35,28.75,26.)) ;
#8149 = CARTESIAN_POINT('',(-6.35,28.75,33.2188933909875)) ;
#8150 = CARTESIAN_POINT('',(-6.325,28.75,33.2190476190476)) ;
#8151 = CARTESIAN_POINT('Origin',(-6.325,28.75,28.2440359709998)) ;
#8152 = CARTESIAN_POINT('',(-6.35,28.75,26.)) ;
#8153 = CARTESIAN_POINT('',(-6.35,28.75,26.)) ;
#8154 = CARTESIAN_POINT('',(6.35,28.75,26.)) ;
#8155 = CARTESIAN_POINT('',(-6.35,28.75,26.)) ;
#8156 = CARTESIAN_POINT('',(6.35,28.75,33.2188933909875)) ;
#8157 = CARTESIAN_POINT('',(6.35,28.75,26.)) ;
#8158 = CARTESIAN_POINT('',(6.325,28.75,33.2190476190476)) ;
#8159 = CARTESIAN_POINT('Origin',(6.325,28.75,28.2440359709998)) ;
#8160 = CARTESIAN_POINT('',(-7.925,28.75,33.2190476190476)) ;
#8161 = CARTESIAN_POINT('Origin',(6.35,14.875,7.)) ;
#8162 = CARTESIAN_POINT('',(6.35,28.5998549795853,33.4000207172021)) ;
#8163 = CARTESIAN_POINT('',(6.35,35.4862056496714,25.0926770517013)) ;
#8164 = CARTESIAN_POINT('',(6.35,28.,22.2)) ;
#8165 = CARTESIAN_POINT('',(6.35,28.,22.2)) ;
#8166 = CARTESIAN_POINT('',(6.35,15.25,-20.)) ;
#8167 = CARTESIAN_POINT('',(6.35,15.25,-20.)) ;
#8168 = CARTESIAN_POINT('',(6.35,1.,-20.)) ;
#8169 = CARTESIAN_POINT('',(6.35,1.,-20.)) ;
#8170 = CARTESIAN_POINT('',(6.35,1.,33.5)) ;
#8171 = CARTESIAN_POINT('',(6.35,1.,34.)) ;
#8172 = CARTESIAN_POINT('',(6.35,27.9,33.5)) ;
#8173 = CARTESIAN_POINT('',(6.35,7.4375,33.5)) ;
#8174 = CARTESIAN_POINT('',(6.35,23.72275,34.09675)) ;
#8175 = CARTESIAN_POINT('Origin',(-6.35,28.,22.2)) ;
#8176 = CARTESIAN_POINT('',(-6.35,28.,22.2)) ;
#8177 = CARTESIAN_POINT('',(-6.35,28.,22.2)) ;
#8178 = CARTESIAN_POINT('',(-6.35,28.,22.2)) ;
#8179 = CARTESIAN_POINT('Origin',(-6.35,15.25,-20.)) ;
#8180 = CARTESIAN_POINT('',(-6.35,15.25,-20.)) ;
#8181 = CARTESIAN_POINT('',(-6.35,15.25,-20.)) ;
#8182 = CARTESIAN_POINT('',(-6.35,15.25,-20.)) ;
#8183 = CARTESIAN_POINT('Origin',(-6.35,1.,-20.)) ;
#8184 = CARTESIAN_POINT('',(-6.35,1.,-20.)) ;
#8185 = CARTESIAN_POINT('',(-6.35,1.,-20.)) ;
#8186 = CARTESIAN_POINT('',(-6.35,1.,-20.)) ;
#8187 = CARTESIAN_POINT('Origin',(-6.35,1.,34.)) ;
#8188 = CARTESIAN_POINT('',(-6.35,1.,33.5)) ;
#8189 = CARTESIAN_POINT('',(-15.425,1.,33.5)) ;
#8190 = CARTESIAN_POINT('',(-6.35,1.,34.)) ;
#8191 = CARTESIAN_POINT('Origin',(-6.35,14.875,7.)) ;
#8192 = CARTESIAN_POINT('',(-6.35,28.5998549795853,33.4000207172021)) ;
#8193 = CARTESIAN_POINT('',(-6.35,35.4862056496714,25.0926770517013)) ;
#8194 = CARTESIAN_POINT('',(-6.35,27.9,33.5)) ;
#8195 = CARTESIAN_POINT('',(-6.35,23.72275,34.09675)) ;
#8196 = CARTESIAN_POINT('',(-6.35,7.4375,33.5)) ;
#8197 = CARTESIAN_POINT('Origin',(-9.5,31.75,29.6)) ;
#8198 = CARTESIAN_POINT('',(6.325,31.75,29.6)) ;
#8199 = CARTESIAN_POINT('',(6.325,35.4862814263725,25.0927398665982)) ;
#8200 = CARTESIAN_POINT('',(-6.325,31.75,29.6)) ;
#8201 = CARTESIAN_POINT('',(-9.5,31.75,29.6)) ;
#8202 = CARTESIAN_POINT('',(-6.325,35.4862814263725,25.0927398665982)) ;
#8203 = CARTESIAN_POINT('Origin',(6.325,33.0419144924728,23.0664883292866)) ;
#8204 = CARTESIAN_POINT('',(6.8058099585235,28.5460488256182,33.407707310626)) ;
#8205 = CARTESIAN_POINT('Origin',(6.325,23.9220039727312,34.0682851467527)) ;
#8206 = CARTESIAN_POINT('',(9.5,24.6003192917499,33.25)) ;
#8207 = CARTESIAN_POINT('Origin',(6.325,24.6003192917499,33.25)) ;
#8208 = CARTESIAN_POINT('',(9.5,28.575,28.4551470821109)) ;
#8209 = CARTESIAN_POINT('',(9.5,33.0419144924728,23.0664883292866)) ;
#8210 = CARTESIAN_POINT('Origin',(6.325,28.575,28.4551470821109)) ;
#8211 = CARTESIAN_POINT('Origin',(-9.5,28.6,33.4)) ;
#8212 = CARTESIAN_POINT('',(7.77490213744257,27.9,33.5)) ;
#8213 = CARTESIAN_POINT('',(-9.5,27.9,33.5)) ;
#8214 = CARTESIAN_POINT('Ctrl Pts',(6.80580995852343,28.5460488256182,33.407707310626)) ;
#8215 = CARTESIAN_POINT('Ctrl Pts',(6.98149608419224,28.5063917103341,33.4133726128094)) ;
#8216 = CARTESIAN_POINT('Ctrl Pts',(7.15246189889731,28.4448215928176,33.4221683438834)) ;
#8217 = CARTESIAN_POINT('Ctrl Pts',(7.51422463753846,28.257594890715,33.4489150156123)) ;
#8218 = CARTESIAN_POINT('Ctrl Pts',(7.65963613230187,28.138247635494,33.4659646235008)) ;
#8219 = CARTESIAN_POINT('Ctrl Pts',(7.77111347508396,28.0136205242995,33.4837684965286)) ;
#8220 = CARTESIAN_POINT('Ctrl Pts',(7.79340206880744,27.9818131636569,33.4883124051919)) ;
#8221 = CARTESIAN_POINT('Ctrl Pts',(7.80749608791706,27.9495759565561,33.492917720492)) ;
#8222 = CARTESIAN_POINT('Ctrl Pts',(7.81039840242134,27.9412633965255,33.4941052290678)) ;
#8223 = CARTESIAN_POINT('Ctrl Pts',(7.81205507027208,27.9288342740703,33.49588081799)) ;
#8224 = CARTESIAN_POINT('Ctrl Pts',(7.81211175307097,27.9241339804662,33.4965522885068)) ;
#8225 = CARTESIAN_POINT('Ctrl Pts',(7.81035146711017,27.9167681745698,33.497604546492)) ;
#8226 = CARTESIAN_POINT('Ctrl Pts',(7.80915473049808,27.9140001175515,33.4979999832069)) ;
#8227 = CARTESIAN_POINT('Ctrl Pts',(7.80568132004777,27.9092451830197,33.4986792595686)) ;
#8228 = CARTESIAN_POINT('Ctrl Pts',(7.80360341728409,27.907368861679,33.4989473054744)) ;
#8229 = CARTESIAN_POINT('Ctrl Pts',(7.79812049420868,27.9038813555221,33.4994455206397)) ;
#8230 = CARTESIAN_POINT('Ctrl Pts',(7.79461677020034,27.902571843467,33.4996325937904)) ;
#8231 = CARTESIAN_POINT('Ctrl Pts',(7.78586974385829,27.9004243166327,33.4999393833382)) ;
#8232 = CARTESIAN_POINT('Ctrl Pts',(7.78023927099663,27.9,33.5)) ;
#8233 = CARTESIAN_POINT('Ctrl Pts',(7.77490213744257,27.9,33.5)) ;
#8234 = CARTESIAN_POINT('Origin',(-18.25,3.05,10.325)) ;
#8235 = CARTESIAN_POINT('',(-18.25,3.3,13.24)) ;
#8236 = CARTESIAN_POINT('',(-18.25,3.05,12.99)) ;
#8237 = CARTESIAN_POINT('Origin',(-18.25,3.05,13.24)) ;
#8238 = CARTESIAN_POINT('',(-18.25,3.05,7.66)) ;
#8239 = CARTESIAN_POINT('Origin',(-18.25,3.05,10.325)) ;
#8240 = CARTESIAN_POINT('',(-18.25,3.3,7.41)) ;
#8241 = CARTESIAN_POINT('Origin',(-18.25,3.05,7.41)) ;
#8242 = CARTESIAN_POINT('Origin',(-18.25,3.3,10.325)) ;
#8243 = CARTESIAN_POINT('Origin',(-9.12502074844716,3.05,7.41)) ;
#8244 = CARTESIAN_POINT('',(-16.75,3.05,7.66)) ;
#8245 = CARTESIAN_POINT('',(-16.75,3.3,7.41)) ;
#8246 = CARTESIAN_POINT('Origin',(-16.75,3.05,7.41)) ;
#8247 = CARTESIAN_POINT('',(-9.12502074844716,3.3,7.41)) ;
#8248 = CARTESIAN_POINT('',(-9.12502074844716,3.05,7.66)) ;
#8249 = CARTESIAN_POINT('Origin',(-16.75,3.05,10.325)) ;
#8250 = CARTESIAN_POINT('',(-16.75,3.05,12.99)) ;
#8251 = CARTESIAN_POINT('',(-16.75,3.3,13.24)) ;
#8252 = CARTESIAN_POINT('Origin',(-16.75,3.05,13.24)) ;
#8253 = CARTESIAN_POINT('Origin',(-16.75,3.3,10.325)) ;
#8254 = CARTESIAN_POINT('Origin',(-16.75,3.05,10.325)) ;
#8255 = CARTESIAN_POINT('Origin',(-8.37502074844716,3.05,13.24)) ;
#8256 = CARTESIAN_POINT('',(-8.37502074844716,3.3,13.24)) ;
#8257 = CARTESIAN_POINT('',(-8.37502074844716,3.05,12.99)) ;
#8258 = CARTESIAN_POINT('Origin',(-18.25,0.,7.66)) ;
#8259 = CARTESIAN_POINT('',(-18.25,0.,7.66)) ;
#8260 = CARTESIAN_POINT('',(-18.25,0.,7.66)) ;
#8261 = CARTESIAN_POINT('',(-16.75,0.,7.66)) ;
#8262 = CARTESIAN_POINT('',(-16.75,0.,7.66)) ;
#8263 = CARTESIAN_POINT('',(-16.75,0.,7.66)) ;
#8264 = CARTESIAN_POINT('Origin',(-18.25,0.,10.325)) ;
#8265 = CARTESIAN_POINT('',(-18.25,0.,12.99)) ;
#8266 = CARTESIAN_POINT('',(-18.25,0.,12.99)) ;
#8267 = CARTESIAN_POINT('Origin',(-18.25,0.,10.325)) ;
#8268 = CARTESIAN_POINT('Origin',(-4.14968943118765E-5,3.3,0.0099999999999989)) ;
#8269 = CARTESIAN_POINT('',(-11.5234336016174,3.3,-28.4730130039621)) ;
#8270 = CARTESIAN_POINT('',(-10.77,3.3,-29.176932678781)) ;
#8271 = CARTESIAN_POINT('Origin',(1.11022302462516E-15,3.3,-16.8941925465839)) ;
#8272 = CARTESIAN_POINT('',(-23.6251157417011,3.3,-16.3713308677057)) ;
#8273 = CARTESIAN_POINT('',(-15.7632336789269,3.3,-24.2332129304798)) ;
#8274 = CARTESIAN_POINT('',(-24.4999998519293,3.3,-14.3009167753159)) ;
#8275 = CARTESIAN_POINT('Origin',(-21.664129241231,3.3,-14.3226323462975)) ;
#8276 = CARTESIAN_POINT('',(-24.5,3.3,33.25)) ;
#8277 = CARTESIAN_POINT('',(-24.5,3.3,-7.145)) ;
#8278 = CARTESIAN_POINT('',(-10.77,3.3,33.25)) ;
#8279 = CARTESIAN_POINT('',(-12.2500207484472,3.3,33.25)) ;
#8280 = CARTESIAN_POINT('',(-10.77,3.3,1.2425)) ;
#8281 = CARTESIAN_POINT('',(-18.25,3.3,-8.985)) ;
#8282 = CARTESIAN_POINT('Origin',(-18.25,3.3,-11.9)) ;
#8283 = CARTESIAN_POINT('Origin',(-18.25,3.05,-11.9)) ;
#8284 = CARTESIAN_POINT('',(-18.25,3.05,-9.235)) ;
#8285 = CARTESIAN_POINT('Origin',(-18.25,3.05,-8.985)) ;
#8286 = CARTESIAN_POINT('',(-20.915,3.05,-11.9)) ;
#8287 = CARTESIAN_POINT('Origin',(-18.25,3.05,-11.9)) ;
#8288 = CARTESIAN_POINT('Origin',(-18.25,3.05,-11.9)) ;
#8289 = CARTESIAN_POINT('Origin',(-18.25,0.,-11.9)) ;
#8290 = CARTESIAN_POINT('',(-20.915,0.,-11.9)) ;
#8291 = CARTESIAN_POINT('',(-20.915,0.,-11.9)) ;
#8292 = CARTESIAN_POINT('Origin',(-18.25,0.,-11.9)) ;
#8293 = CARTESIAN_POINT('Origin',(18.25,3.05,-11.9)) ;
#8294 = CARTESIAN_POINT('',(18.25,3.3,-8.985)) ;
#8295 = CARTESIAN_POINT('Origin',(18.25,3.3,-11.9)) ;
#8296 = CARTESIAN_POINT('',(18.25,3.05,-9.235)) ;
#8297 = CARTESIAN_POINT('Origin',(18.25,3.05,-8.985)) ;
#8298 = CARTESIAN_POINT('',(15.585,3.05,-11.9)) ;
#8299 = CARTESIAN_POINT('Origin',(18.25,3.05,-11.9)) ;
#8300 = CARTESIAN_POINT('Origin',(18.25,3.05,-11.9)) ;
#8301 = CARTESIAN_POINT('Origin',(-4.14968943118765E-5,3.3,0.0099999999999989)) ;
#8302 = CARTESIAN_POINT('',(24.5,3.3,33.25)) ;
#8303 = CARTESIAN_POINT('',(10.77,3.3,33.25)) ;
#8304 = CARTESIAN_POINT('',(-12.2500207484472,3.3,33.25)) ;
#8305 = CARTESIAN_POINT('',(24.5,3.3,-14.2973164482764)) ;
#8306 = CARTESIAN_POINT('',(24.5,3.3,16.63)) ;
#8307 = CARTESIAN_POINT('',(23.6225672795876,3.3,-16.373879130817)) ;
#8308 = CARTESIAN_POINT('Origin',(21.4457388066382,3.3,-14.2304230516917)) ;
#8309 = CARTESIAN_POINT('',(11.5234336029266,3.3,-28.4730130064801)) ;
#8310 = CARTESIAN_POINT('',(21.8132129304798,3.3,-18.1832336789269)) ;
#8311 = CARTESIAN_POINT('',(10.77,3.3,-29.176932678781)) ;
#8312 = CARTESIAN_POINT('Origin',(1.11022302462516E-15,3.3,-16.8941925465839)) ;
#8313 = CARTESIAN_POINT('',(10.77,3.3,1.2425)) ;
#8314 = CARTESIAN_POINT('',(16.75,3.3,7.41)) ;
#8315 = CARTESIAN_POINT('',(16.75,3.3,13.24)) ;
#8316 = CARTESIAN_POINT('Origin',(16.75,3.3,10.325)) ;
#8317 = CARTESIAN_POINT('',(18.25,3.3,7.41)) ;
#8318 = CARTESIAN_POINT('',(8.37497925155284,3.3,7.41)) ;
#8319 = CARTESIAN_POINT('',(18.25,3.3,13.24)) ;
#8320 = CARTESIAN_POINT('Origin',(18.25,3.3,10.325)) ;
#8321 = CARTESIAN_POINT('',(9.12497925155284,3.3,13.24)) ;
#8322 = CARTESIAN_POINT('Origin',(18.25,0.,-11.9)) ;
#8323 = CARTESIAN_POINT('',(15.585,0.,-11.9)) ;
#8324 = CARTESIAN_POINT('',(15.585,0.,-11.9)) ;
#8325 = CARTESIAN_POINT('Origin',(18.25,0.,-11.9)) ;
#8326 = CARTESIAN_POINT('Origin',(16.75,3.05,10.325)) ;
#8327 = CARTESIAN_POINT('',(16.75,3.05,12.99)) ;
#8328 = CARTESIAN_POINT('Origin',(16.75,3.05,13.24)) ;
#8329 = CARTESIAN_POINT('',(16.75,3.05,7.66)) ;
#8330 = CARTESIAN_POINT('Origin',(16.75,3.05,10.325)) ;
#8331 = CARTESIAN_POINT('Origin',(16.75,3.05,7.41)) ;
#8332 = CARTESIAN_POINT('Origin',(8.37497925155284,3.05,7.41)) ;
#8333 = CARTESIAN_POINT('',(18.25,3.05,7.66)) ;
#8334 = CARTESIAN_POINT('Origin',(18.25,3.05,7.41)) ;
#8335 = CARTESIAN_POINT('',(8.37497925155284,3.05,7.66)) ;
#8336 = CARTESIAN_POINT('Origin',(18.25,3.05,10.325)) ;
#8337 = CARTESIAN_POINT('',(18.25,3.05,12.99)) ;
#8338 = CARTESIAN_POINT('Origin',(18.25,3.05,13.24)) ;
#8339 = CARTESIAN_POINT('Origin',(18.25,3.05,10.325)) ;
#8340 = CARTESIAN_POINT('Origin',(9.12497925155284,3.05,13.24)) ;
#8341 = CARTESIAN_POINT('',(9.12497925155284,3.05,12.99)) ;
#8342 = CARTESIAN_POINT('Origin',(16.75,0.,7.66)) ;
#8343 = CARTESIAN_POINT('',(16.75,0.,7.66)) ;
#8344 = CARTESIAN_POINT('',(16.75,0.,7.66)) ;
#8345 = CARTESIAN_POINT('',(18.25,0.,7.66)) ;
#8346 = CARTESIAN_POINT('',(18.25,0.,7.66)) ;
#8347 = CARTESIAN_POINT('',(18.25,0.,7.66)) ;
#8348 = CARTESIAN_POINT('Origin',(16.75,0.,10.325)) ;
#8349 = CARTESIAN_POINT('',(16.75,0.,12.99)) ;
#8350 = CARTESIAN_POINT('',(16.75,0.,12.99)) ;
#8351 = CARTESIAN_POINT('Origin',(16.75,0.,10.325)) ;
#8352 = CARTESIAN_POINT('Ctrl Pts',(6.76795090667119,28.3557987366091,33.5)) ;
#8353 = CARTESIAN_POINT('Ctrl Pts',(7.54929504861544,28.2003141923527,33.5)) ;
#8354 = CARTESIAN_POINT('Ctrl Pts',(8.81719996776912,27.1694431484449,33.5)) ;
#8355 = CARTESIAN_POINT('Ctrl Pts',(9.25,25.370369005669,33.5)) ;
#8356 = CARTESIAN_POINT('Ctrl Pts',(9.25,24.6003192917499,33.5)) ;
#8357 = CARTESIAN_POINT('Ctrl Pts',(6.77517359820442,28.3920943552222,33.5)) ;
#8358 = CARTESIAN_POINT('Ctrl Pts',(7.5693362493457,28.2354900210942,33.5000078650668)) ;
#8359 = CARTESIAN_POINT('Ctrl Pts',(8.85942127194598,27.1975612821968,33.4998356946794)) ;
#8360 = CARTESIAN_POINT('Ctrl Pts',(9.31001237129095,25.3805985297588,33.4998240176448)) ;
#8361 = CARTESIAN_POINT('Ctrl Pts',(9.31544984694979,24.6003192917499,33.5)) ;
#8362 = CARTESIAN_POINT('Ctrl Pts',(6.78961185129094,28.464649762726,33.483268532741)) ;
#8363 = CARTESIAN_POINT('Ctrl Pts',(7.60938939076488,28.3057987139221,33.4819757476224)) ;
#8364 = CARTESIAN_POINT('Ctrl Pts',(8.94398652948134,27.2537008535442,33.4736901555626)) ;
#8365 = CARTESIAN_POINT('Ctrl Pts',(9.42982991123221,25.4008861366219,33.4551270066274)) ;
#8366 = CARTESIAN_POINT('Ctrl Pts',(9.4456714379219,24.6003192917499,33.4456714379219)) ;
#8367 = CARTESIAN_POINT('Ctrl Pts',(6.80125367349468,28.5231524880223,33.4364220663262)) ;
#8368 = CARTESIAN_POINT('Ctrl Pts',(7.64149663567339,28.3614500536775,33.4317712233585)) ;
#8369 = CARTESIAN_POINT('Ctrl Pts',(9.00760901658297,27.2899950446832,33.4011943379152)) ;
#8370 = CARTESIAN_POINT('Ctrl Pts',(9.49134428057035,25.4094606950313,33.342417324315)) ;
#8371 = CARTESIAN_POINT('Ctrl Pts',(9.5,24.6003192917499,33.3154498469498)) ;
#8372 = CARTESIAN_POINT('Ctrl Pts',(6.80580995852343,28.5460488256182,33.407707310626)) ;
#8373 = CARTESIAN_POINT('Ctrl Pts',(7.6539356510612,28.3826875378412,33.4011779048128)) ;
#8374 = CARTESIAN_POINT('Ctrl Pts',(9.0302085120229,27.2995932530023,33.3578875866726)) ;
#8375 = CARTESIAN_POINT('Ctrl Pts',(9.5,25.4093792116268,33.2823374075703)) ;
#8376 = CARTESIAN_POINT('Ctrl Pts',(9.5,24.6003192917499,33.25)) ;
#8377 = CARTESIAN_POINT('',(9.25,24.6003192917499,33.5)) ;
#8378 = CARTESIAN_POINT('Origin',(6.325,24.6003192917499,33.5)) ;
#8379 = CARTESIAN_POINT('Origin',(9.25,24.6003192917499,33.25)) ;
#8380 = CARTESIAN_POINT('Origin',(9.25,8.6875,33.25)) ;
#8381 = CARTESIAN_POINT('',(9.25,4.57,33.5)) ;
#8382 = CARTESIAN_POINT('',(9.5,4.57,33.25)) ;
#8383 = CARTESIAN_POINT('Origin',(9.25,4.57,33.25)) ;
#8384 = CARTESIAN_POINT('',(9.5,8.6875,33.25)) ;
#8385 = CARTESIAN_POINT('',(9.25,8.6875,33.5)) ;
#8386 = CARTESIAN_POINT('Origin',(-12.2500207484472,3.05,33.25)) ;
#8387 = CARTESIAN_POINT('',(10.77,3.05,33.5)) ;
#8388 = CARTESIAN_POINT('Origin',(10.77,3.05,33.25)) ;
#8389 = CARTESIAN_POINT('',(24.5,3.05,33.5)) ;
#8390 = CARTESIAN_POINT('',(-12.2500207484472,3.05,33.5)) ;
#8391 = CARTESIAN_POINT('Origin',(24.5,3.05,33.25)) ;
#8392 = CARTESIAN_POINT('Origin',(10.77,4.57,33.25)) ;
#8393 = CARTESIAN_POINT('Origin',(10.77,4.57,33.25)) ;
#8394 = CARTESIAN_POINT('Origin',(10.77,4.57,33.5)) ;
#8395 = CARTESIAN_POINT('Origin',(21.4457388066382,3.05,-14.2304230516917)) ;
#8396 = CARTESIAN_POINT('',(24.75,3.05,-14.3)) ;
#8397 = CARTESIAN_POINT('',(23.8,3.05,-16.55)) ;
#8398 = CARTESIAN_POINT('Origin',(21.4457388066382,3.05,-14.2304230516917)) ;
#8399 = CARTESIAN_POINT('Ctrl Pts',(23.8,3.05,-16.55)) ;
#8400 = CARTESIAN_POINT('Ctrl Pts',(23.8000293456249,3.06636246173745,-16.5499702155749)) ;
#8401 = CARTESIAN_POINT('Ctrl Pts',(23.798910747616,3.08272451888078,-16.5488094001891)) ;
#8402 = CARTESIAN_POINT('Ctrl Pts',(23.7966660800154,3.09877258050403,-16.5465393599234)) ;
#8403 = CARTESIAN_POINT('Ctrl Pts',(23.7945144670797,3.11415535565185,-16.5443634261687)) ;
#8404 = CARTESIAN_POINT('Ctrl Pts',(23.7913285774613,3.12924901836754,-16.5411686882304)) ;
#8405 = CARTESIAN_POINT('Ctrl Pts',(23.7871649259446,3.1437876509661,-16.5370110383706)) ;
#8406 = CARTESIAN_POINT('Ctrl Pts',(23.7830020587907,3.15832354472801,-16.5328541717429)) ;
#8407 = CARTESIAN_POINT('Ctrl Pts',(23.7778619736653,3.17230401141269,-16.5277349297353)) ;
#8408 = CARTESIAN_POINT('Ctrl Pts',(23.7718355851639,3.18548283774181,-16.5217430712642)) ;
#8409 = CARTESIAN_POINT('Ctrl Pts',(23.765810164708,3.19865954709755,-16.5157521752919)) ;
#8410 = CARTESIAN_POINT('Ctrl Pts',(23.7588989785171,3.21103432480559,-16.5088891930629)) ;
#8411 = CARTESIAN_POINT('Ctrl Pts',(23.7512241009886,3.22238930539324,-16.5012745467355)) ;
#8412 = CARTESIAN_POINT('Ctrl Pts',(23.7435502435946,3.23374277669204,-16.4936609125367)) ;
#8413 = CARTESIAN_POINT('Ctrl Pts',(23.7351132191597,3.24407624949196,-16.4852961311533)) ;
#8414 = CARTESIAN_POINT('Ctrl Pts',(23.7260619356313,3.25320784483669,-16.4763270162031)) ;
#8415 = CARTESIAN_POINT('Ctrl Pts',(23.7170075012856,3.26234261895575,-16.4673547790392)) ;
#8416 = CARTESIAN_POINT('Ctrl Pts',(23.7073387574172,3.27027429523935,-16.457778159615)) ;
#8417 = CARTESIAN_POINT('Ctrl Pts',(23.6972264211279,3.27686317193747,-16.4477654057518)) ;
#8418 = CARTESIAN_POINT('Ctrl Pts',(23.6871172241685,3.28345000314799,-16.4377557603037)) ;
#8419 = CARTESIAN_POINT('Ctrl Pts',(23.6765651334693,3.28869459613384,-16.4273106684178)) ;
#8420 = CARTESIAN_POINT('Ctrl Pts',(23.6657563222244,3.2925046341702,-16.4166135482745)) ;
#8421 = CARTESIAN_POINT('Ctrl Pts',(23.6549466148759,3.29631498807748,-16.4059155412874)) ;
#8422 = CARTESIAN_POINT('Ctrl Pts',(23.6438805959438,3.29869038961342,-16.3949659091188)) ;
#8423 = CARTESIAN_POINT('Ctrl Pts',(23.6327535307763,3.29958901942994,-16.3839569688262)) ;
#8424 = CARTESIAN_POINT('Ctrl Pts',(23.6293618826288,3.29986293138305,-16.3806013264006)) ;
#8425 = CARTESIAN_POINT('Ctrl Pts',(23.625964600032,3.3,-16.3772402100488)) ;
#8426 = CARTESIAN_POINT('Ctrl Pts',(23.6225672795876,3.3,-16.373879130817)) ;
#8427 = CARTESIAN_POINT('Ctrl Pts',(24.5,3.3,-14.2973164482764)) ;
#8428 = CARTESIAN_POINT('Ctrl Pts',(24.5015396345052,3.3,-14.2973333065323)) ;
#8429 = CARTESIAN_POINT('Ctrl Pts',(24.5030792362479,3.29998577715355,-14.297350158057)) ;
#8430 = CARTESIAN_POINT('Ctrl Pts',(24.5367196937611,3.29936418270175,-14.2977182266959)) ;
#8431 = CARTESIAN_POINT('Ctrl Pts',(24.5684081693065,3.29259261132557,-14.2980620867652)) ;
#8432 = CARTESIAN_POINT('Ctrl Pts',(24.6278990054925,3.26725920437385,-14.2987032837107)) ;
#8433 = CARTESIAN_POINT('Ctrl Pts',(24.6550726110038,3.24877687466915,-14.2989938308607)) ;
#8434 = CARTESIAN_POINT('Ctrl Pts',(24.7008047506126,3.20243716760779,-14.2994805987249)) ;
#8435 = CARTESIAN_POINT('Ctrl Pts',(24.7189265638722,3.17502334972294,-14.2996722340112)) ;
#8436 = CARTESIAN_POINT('Ctrl Pts',(24.7436421992149,3.11479271760787,-14.2999331603654)) ;
#8437 = CARTESIAN_POINT('Ctrl Pts',(24.75,3.08255201651694,-14.3)) ;
#8438 = CARTESIAN_POINT('Ctrl Pts',(24.75,3.05,-14.3)) ;
#8439 = CARTESIAN_POINT('Origin',(-21.664129241231,3.05,-14.3226323462975)) ;
#8440 = CARTESIAN_POINT('',(-24.75,3.05,-14.3)) ;
#8441 = CARTESIAN_POINT('Ctrl Pts',(-24.75,3.05,-14.3)) ;
#8442 = CARTESIAN_POINT('Ctrl Pts',(-24.7499996951622,3.06636246173745,-14.2999584360325)) ;
#8443 = CARTESIAN_POINT('Ctrl Pts',(-24.7483879108569,3.08272451888078,-14.2999286913692)) ;
#8444 = CARTESIAN_POINT('Ctrl Pts',(-24.745195533686,3.09877258050403,-14.2999107323432)) ;
#8445 = CARTESIAN_POINT('Ctrl Pts',(-24.7421354993356,3.11415535553231,-14.2998935178246)) ;
#8446 = CARTESIAN_POINT('Ctrl Pts',(-24.7376237166988,3.12924901813298,-14.2998871289039)) ;
#8447 = CARTESIAN_POINT('Ctrl Pts',(-24.7317396696698,3.14378765062717,-14.2998911419599)) ;
#8448 = CARTESIAN_POINT('Ctrl Pts',(-24.7258567310994,3.15832354427998,-14.2998951542599)) ;
#8449 = CARTESIAN_POINT('Ctrl Pts',(-24.7186022921447,3.17230401086657,-14.2999095634098)) ;
#8450 = CARTESIAN_POINT('Ctrl Pts',(-24.7101041084036,3.18548283711434,-14.299933571763)) ;
#8451 = CARTESIAN_POINT('Ctrl Pts',(-24.7016072897667,3.19865954638359,-14.2999575762596)) ;
#8452 = CARTESIAN_POINT('Ctrl Pts',(-24.6918674814275,3.21103432402251,-14.2999911747909)) ;
#8453 = CARTESIAN_POINT('Ctrl Pts',(-24.6810561544944,3.22238930456332,-14.3000332206547)) ;
#8454 = CARTESIAN_POINT('Ctrl Pts',(-24.6702462645928,3.23374277581057,-14.3000752609299)) ;
#8455 = CARTESIAN_POINT('Ctrl Pts',(-24.6583655923458,3.24407624858209,-14.3001257433967)) ;
#8456 = CARTESIAN_POINT('Ctrl Pts',(-24.6456232446371,3.25320784392526,-14.3001832098595)) ;
#8457 = CARTESIAN_POINT('Ctrl Pts',(-24.6328764612318,3.26234261803794,-14.3002406963268)) ;
#8458 = CARTESIAN_POINT('Ctrl Pts',(-24.6192679322756,3.27027429434331,-14.300305168057)) ;
#8459 = CARTESIAN_POINT('Ctrl Pts',(-24.6050373423276,3.27686317109361,-14.3003749019062)) ;
#8460 = CARTESIAN_POINT('Ctrl Pts',(-24.590811170207,3.28345000235455,-14.3004446141069)) ;
#8461 = CARTESIAN_POINT('Ctrl Pts',(-24.5759639176278,3.28869459542192,-14.300519580942)) ;
#8462 = CARTESIAN_POINT('Ctrl Pts',(-24.5607569253176,3.29250463357125,-14.3005978764304)) ;
#8463 = CARTESIAN_POINT('Ctrl Pts',(-24.5455486722758,3.29631498759076,-14.3006761784098)) ;
#8464 = CARTESIAN_POINT('Ctrl Pts',(-24.529981253701,3.29869038927096,-14.3007578049366)) ;
#8465 = CARTESIAN_POINT('Ctrl Pts',(-24.514328731891,3.29958901926202,-14.3008406917336)) ;
#8466 = CARTESIAN_POINT('Ctrl Pts',(-24.5095576752671,3.29986293132702,-14.3008659565189)) ;
#8467 = CARTESIAN_POINT('Ctrl Pts',(-24.5047787638457,3.3,-14.3008913376992)) ;
#8468 = CARTESIAN_POINT('Ctrl Pts',(-24.4999998519293,3.3,-14.3009167753159)) ;
#8469 = CARTESIAN_POINT('',(-23.8,3.05,-16.55)) ;
#8470 = CARTESIAN_POINT('Ctrl Pts',(-23.6251157417011,3.3,-16.3713308677057)) ;
#8471 = CARTESIAN_POINT('Ctrl Pts',(-23.6262285835138,3.3,-16.372468319203)) ;
#8472 = CARTESIAN_POINT('Ctrl Pts',(-23.6273414052155,3.29998480854004,-16.3736057396723)) ;
#8473 = CARTESIAN_POINT('Ctrl Pts',(-23.6508682580149,3.29934240875891,-16.3976524294703)) ;
#8474 = CARTESIAN_POINT('Ctrl Pts',(-23.6729946612897,3.29257223359693,-16.4202633562148)) ;
#8475 = CARTESIAN_POINT('Ctrl Pts',(-23.7145752356494,3.26725923592507,-16.4627478051389)) ;
#8476 = CARTESIAN_POINT('Ctrl Pts',(-23.7335850472872,3.24877691508736,-16.4821672771834)) ;
#8477 = CARTESIAN_POINT('Ctrl Pts',(-23.7655795153817,3.2024372164242,-16.5148478457573)) ;
#8478 = CARTESIAN_POINT('Ctrl Pts',(-23.7782585885107,3.17502339467209,-16.527796901805)) ;
#8479 = CARTESIAN_POINT('Ctrl Pts',(-23.795551415589,3.11479274608981,-16.5454572885827)) ;
#8480 = CARTESIAN_POINT('Ctrl Pts',(-23.7999999999999,3.0825520303151,-16.5500000000001)) ;
#8481 = CARTESIAN_POINT('Ctrl Pts',(-23.7999999999999,3.05,-16.5500000000001)) ;
#8482 = CARTESIAN_POINT('Origin',(-21.664129241231,3.05,-14.3226323462975)) ;
#8483 = CARTESIAN_POINT('Origin',(-15.7632336789269,3.05,-24.2332129304798)) ;
#8484 = CARTESIAN_POINT('',(-11.7,3.05,-28.65)) ;
#8485 = CARTESIAN_POINT('Ctrl Pts',(-11.5234344017198,3.3,-28.473012207687)) ;
#8486 = CARTESIAN_POINT('Ctrl Pts',(-11.5248174913711,3.3,-28.4743986171271)) ;
#8487 = CARTESIAN_POINT('Ctrl Pts',(-11.5262005335124,3.29997698962268,-28.4757849786368)) ;
#8488 = CARTESIAN_POINT('Ctrl Pts',(-11.549952120929,3.29918654602524,-28.4995935660478)) ;
#8489 = CARTESIAN_POINT('Ctrl Pts',(-11.5720185826081,3.29242837602069,-28.5217129029688)) ;
#8490 = CARTESIAN_POINT('Ctrl Pts',(-11.6137589203919,3.26726387118117,-28.5635531294894)) ;
#8491 = CARTESIAN_POINT('Ctrl Pts',(-11.6329511205585,3.24878239907981,-28.5827911879915)) ;
#8492 = CARTESIAN_POINT('Ctrl Pts',(-11.6652519474713,3.2024434132778,-28.6151691262904)) ;
#8493 = CARTESIAN_POINT('Ctrl Pts',(-11.6780517643173,3.17502893211547,-28.62799946099)) ;
#8494 = CARTESIAN_POINT('Ctrl Pts',(-11.6955092411612,3.11479613681779,-28.6454985466271)) ;
#8495 = CARTESIAN_POINT('Ctrl Pts',(-11.7,3.08255368454758,-28.65)) ;
#8496 = CARTESIAN_POINT('Ctrl Pts',(-11.7,3.05,-28.65)) ;
#8497 = CARTESIAN_POINT('',(-15.9400103742236,3.05,-24.4099896257764)) ;
#8498 = CARTESIAN_POINT('Ctrl Pts',(10.4512438343541,3.34065281272427,-29.501243923759)) ;
#8499 = CARTESIAN_POINT('Ctrl Pts',(10.5574497695917,3.31311478519587,-29.3965002427796)) ;
#8500 = CARTESIAN_POINT('Ctrl Pts',(10.6644750033045,3.3,-29.2876755180677)) ;
#8501 = CARTESIAN_POINT('Ctrl Pts',(10.77,3.3,-29.176932678781)) ;
#8502 = CARTESIAN_POINT('Ctrl Pts',(10.4867185411393,3.33145461255,-29.5471888940564)) ;
#8503 = CARTESIAN_POINT('Ctrl Pts',(10.5959487962567,3.30645872447267,-29.4433768078905)) ;
#8504 = CARTESIAN_POINT('Ctrl Pts',(10.7056436255396,3.29633423430578,-29.3355995974396)) ;
#8505 = CARTESIAN_POINT('Ctrl Pts',(10.8131502913865,3.3,-29.2261438037327)) ;
#8506 = CARTESIAN_POINT('Ctrl Pts',(10.5465724667282,3.27117973026827,-29.6387913916651)) ;
#8507 = CARTESIAN_POINT('Ctrl Pts',(10.6646000202358,3.24691483243654,-29.5367571598192)) ;
#8508 = CARTESIAN_POINT('Ctrl Pts',(10.7830438290637,3.2389968774968,-29.4311063020666)) ;
#8509 = CARTESIAN_POINT('Ctrl Pts',(10.8990265225851,3.24570588944608,-29.3240820981936)) ;
#8510 = CARTESIAN_POINT('Ctrl Pts',(10.5563795789494,3.15628364564047,-29.6868463778552)) ;
#8511 = CARTESIAN_POINT('Ctrl Pts',(10.6826104679429,3.12626473336083,-29.5827439357331)) ;
#8512 = CARTESIAN_POINT('Ctrl Pts',(10.8096178153565,3.11314703296705,-29.4745902410339)) ;
#8513 = CARTESIAN_POINT('Ctrl Pts',(10.9348219720805,3.11544984694979,-29.3649053297691)) ;
#8514 = CARTESIAN_POINT('Ctrl Pts',(10.5474800757194,3.09865533491409,-29.6941797705656)) ;
#8515 = CARTESIAN_POINT('Ctrl Pts',(10.6765379977093,3.06569643582498,-29.587833112793)) ;
#8516 = CARTESIAN_POINT('Ctrl Pts',(10.8065915039711,3.05,-29.4773429557935)) ;
#8517 = CARTESIAN_POINT('Ctrl Pts',(10.9348219720805,3.05,-29.3649053297691)) ;
#8518 = CARTESIAN_POINT('',(10.4512438329193,3.34065280720824,-29.5012439237535)) ;
#8519 = CARTESIAN_POINT('Ctrl Pts',(10.4512438343541,3.34065281272427,-29.501243923759)) ;
#8520 = CARTESIAN_POINT('Ctrl Pts',(10.5574497695917,3.31311478519587,-29.3965002427796)) ;
#8521 = CARTESIAN_POINT('Ctrl Pts',(10.6644750033045,3.3,-29.2876755180677)) ;
#8522 = CARTESIAN_POINT('Ctrl Pts',(10.77,3.3,-29.176932678781)) ;
#8523 = CARTESIAN_POINT('',(10.9348219720805,3.05,-29.3649053297691)) ;
#8524 = CARTESIAN_POINT('Origin',(10.77,3.05,-29.176932678781)) ;
#8525 = CARTESIAN_POINT('',(10.5823632225196,3.09017244597965,-29.6653552778491)) ;
#8526 = CARTESIAN_POINT('Ctrl Pts',(10.9348219720805,3.05,-29.3649053297691)) ;
#8527 = CARTESIAN_POINT('Ctrl Pts',(10.8181371295453,3.05,-29.4672192874511)) ;
#8528 = CARTESIAN_POINT('Ctrl Pts',(10.6999427554713,3.06299713058315,-29.5679206810131)) ;
#8529 = CARTESIAN_POINT('Ctrl Pts',(10.5823626153175,3.09017135645643,-29.6653548535384)) ;
#8530 = CARTESIAN_POINT('',(10.4562560925639,3.33923511979837,-29.5067623750852)) ;
#8531 = CARTESIAN_POINT('Ctrl Pts',(10.5823613854325,3.09017164069861,-29.6653558726971)) ;
#8532 = CARTESIAN_POINT('Ctrl Pts',(10.5823677899508,3.09071784580571,-29.6653506827371)) ;
#8533 = CARTESIAN_POINT('Ctrl Pts',(10.5823730307843,3.09126403335751,-29.6653440861951)) ;
#8534 = CARTESIAN_POINT('Ctrl Pts',(10.5823771106453,3.09181019549258,-29.6653360863522)) ;
#8535 = CARTESIAN_POINT('Ctrl Pts',(10.5824953065254,3.10763282149373,-29.6651043263781)) ;
#8536 = CARTESIAN_POINT('Ctrl Pts',(10.581641197747,3.12338319864702,-29.6636993620564)) ;
#8537 = CARTESIAN_POINT('Ctrl Pts',(10.5798821820818,3.13887085021686,-29.6612010522168)) ;
#8538 = CARTESIAN_POINT('Ctrl Pts',(10.5788028689804,3.14837390671523,-29.6596681161581)) ;
#8539 = CARTESIAN_POINT('Ctrl Pts',(10.5773821081474,3.15777816572057,-29.6577227554171)) ;
#8540 = CARTESIAN_POINT('Ctrl Pts',(10.5756284659994,3.16703794902945,-29.6553769789403)) ;
#8541 = CARTESIAN_POINT('Ctrl Pts',(10.5727717533484,3.18212229229376,-29.6515556694758)) ;
#8542 = CARTESIAN_POINT('Ctrl Pts',(10.5690518851304,3.19672783154786,-29.6466977551295)) ;
#8543 = CARTESIAN_POINT('Ctrl Pts',(10.5645156102124,3.21065867009823,-29.640864699056)) ;
#8544 = CARTESIAN_POINT('Ctrl Pts',(10.5617795259203,3.21906114773045,-29.6373464526124)) ;
#8545 = CARTESIAN_POINT('Ctrl Pts',(10.5587457101495,3.22721796960851,-29.6334728036728)) ;
#8546 = CARTESIAN_POINT('Ctrl Pts',(10.5554180283936,3.23508172139697,-29.629252267027)) ;
#8547 = CARTESIAN_POINT('Ctrl Pts',(10.5525046602579,3.24196639534373,-29.6255572090613)) ;
#8548 = CARTESIAN_POINT('Ctrl Pts',(10.54937781422,3.24859840739661,-29.6216111610704)) ;
#8549 = CARTESIAN_POINT('Ctrl Pts',(10.5460432855329,3.2549488825252,-29.6174233243881)) ;
#8550 = CARTESIAN_POINT('Ctrl Pts',(10.5397549905257,3.26692468624192,-29.6095258507203)) ;
#8551 = CARTESIAN_POINT('Ctrl Pts',(10.5327298507231,3.27790178281476,-29.600769706281)) ;
#8552 = CARTESIAN_POINT('Ctrl Pts',(10.5250883209327,3.28777924334128,-29.5912904807446)) ;
#8553 = CARTESIAN_POINT('Ctrl Pts',(10.5209275848499,3.29315742121225,-29.5861291378187)) ;
#8554 = CARTESIAN_POINT('Ctrl Pts',(10.5165835641967,3.29820896154503,-29.5807530157848)) ;
#8555 = CARTESIAN_POINT('Ctrl Pts',(10.5120725594015,3.30291220128229,-29.5751821384144)) ;
#8556 = CARTESIAN_POINT('Ctrl Pts',(10.5036194939666,3.31172549123882,-29.5647430027716)) ;
#8557 = CARTESIAN_POINT('Ctrl Pts',(10.4946636079744,3.31923399426322,-29.5537197514597)) ;
#8558 = CARTESIAN_POINT('Ctrl Pts',(10.4853242585872,3.32533098308598,-29.5422670754818)) ;
#8559 = CARTESIAN_POINT('Ctrl Pts',(10.4759849091999,3.33142797190874,-29.530814399504)) ;
#8560 = CARTESIAN_POINT('Ctrl Pts',(10.4662611466213,3.33611439356466,-29.5189310532188)) ;
#8561 = CARTESIAN_POINT('Ctrl Pts',(10.4562542977309,3.33923061889938,-29.506761629053)) ;
#8562 = CARTESIAN_POINT('Ctrl Pts',(10.4562560925639,3.33923511979837,-29.5067623750852)) ;
#8563 = CARTESIAN_POINT('Ctrl Pts',(10.454686244446,3.33972076841164,-29.5048541775706)) ;
#8564 = CARTESIAN_POINT('Ctrl Pts',(10.4530149306185,3.34019358706778,-29.5030149306185)) ;
#8565 = CARTESIAN_POINT('Ctrl Pts',(10.4512438793665,3.34065280105307,-29.5012438793665)) ;
#8566 = CARTESIAN_POINT('Ctrl Pts',(-10.4562560925639,3.33923511979837,-29.5067623750852)) ;
#8567 = CARTESIAN_POINT('Ctrl Pts',(-10.3042079931798,3.31229863060029,-29.6126005064717)) ;
#8568 = CARTESIAN_POINT('Ctrl Pts',(-10.1477491130449,3.3,-29.7175603525465)) ;
#8569 = CARTESIAN_POINT('Ctrl Pts',(-9.98909940046129,3.3,-29.8200000000001)) ;
#8570 = CARTESIAN_POINT('Ctrl Pts',(-10.4937439232518,3.32847961370675,-29.5490226213438)) ;
#8571 = CARTESIAN_POINT('Ctrl Pts',(-10.3424189419941,3.3045346571375,-29.6585580134996)) ;
#8572 = CARTESIAN_POINT('Ctrl Pts',(-10.1867667904971,3.29572909993472,-29.7667751370844)) ;
#8573 = CARTESIAN_POINT('Ctrl Pts',(-10.0291209928307,3.3,-29.8717875912741)) ;
#8574 = CARTESIAN_POINT('Ctrl Pts',(-10.5685054554551,3.2669079755233,-29.62309040069)) ;
#8575 = CARTESIAN_POINT('Ctrl Pts',(-10.418549761391,3.24402514762918,-29.742418677397)) ;
#8576 = CARTESIAN_POINT('Ctrl Pts',(-10.2645399752037,3.23788937883,-29.8603708829999)) ;
#8577 = CARTESIAN_POINT('Ctrl Pts',(-10.1087705983175,3.24570589574959,-29.9748534857045)) ;
#8578 = CARTESIAN_POINT('Ctrl Pts',(-10.6091727180391,3.15371643721036,-29.6430963665886)) ;
#8579 = CARTESIAN_POINT('Ctrl Pts',(-10.4570254125938,3.1246417608215,-29.7697804551427)) ;
#8580 = CARTESIAN_POINT('Ctrl Pts',(-10.3004417599091,3.11276689086104,-29.8952373576481)) ;
#8581 = CARTESIAN_POINT('Ctrl Pts',(-10.1419706226055,3.11544984694979,-30.01781402741)) ;
#8582 = CARTESIAN_POINT('Ctrl Pts',(-10.6162765892914,3.09695856857757,-29.6371780782973)) ;
#8583 = CARTESIAN_POINT('Ctrl Pts',(-10.4619015755534,3.06471962087594,-29.7657890572739)) ;
#8584 = CARTESIAN_POINT('Ctrl Pts',(-10.3030482793393,3.05,-29.8933327731359)) ;
#8585 = CARTESIAN_POINT('Ctrl Pts',(-10.1419706226054,3.05,-30.01781402741)) ;
#8586 = CARTESIAN_POINT('',(-10.4562560925639,3.33923511979837,-29.5067623750852)) ;
#8587 = CARTESIAN_POINT('',(-9.9890994004613,3.3,-29.82)) ;
#8588 = CARTESIAN_POINT('Ctrl Pts',(-10.4562560925639,3.33923511979837,-29.5067623750852)) ;
#8589 = CARTESIAN_POINT('Ctrl Pts',(-10.3042079931798,3.31229863060029,-29.6126005064717)) ;
#8590 = CARTESIAN_POINT('Ctrl Pts',(-10.1477491130449,3.3,-29.7175603525465)) ;
#8591 = CARTESIAN_POINT('Ctrl Pts',(-9.98909940046129,3.3,-29.8200000000001)) ;
#8592 = CARTESIAN_POINT('',(-10.1419706226054,3.05,-30.01781402741)) ;
#8593 = CARTESIAN_POINT('Origin',(-9.98909940046129,3.05,-29.8200000000001)) ;
#8594 = CARTESIAN_POINT('',(-10.5823632225197,3.09017244597965,-29.6653552778491)) ;
#8595 = CARTESIAN_POINT('Ctrl Pts',(-10.1419706226054,3.05,-30.01781402741)) ;
#8596 = CARTESIAN_POINT('Ctrl Pts',(-10.2912776199237,3.05,-29.902429170969)) ;
#8597 = CARTESIAN_POINT('Ctrl Pts',(-10.4386734667128,3.06264696571335,-29.7844130751078)) ;
#8598 = CARTESIAN_POINT('Ctrl Pts',(-10.582363125788,3.09017060002378,-29.6653547280519)) ;
#8599 = CARTESIAN_POINT('Ctrl Pts',(-10.5823645492884,3.0901708726946,-29.6653535485681)) ;
#8600 = CARTESIAN_POINT('Ctrl Pts',(-10.58237093712,3.09071707945032,-29.6653483728594)) ;
#8601 = CARTESIAN_POINT('Ctrl Pts',(-10.5823761674002,3.09126326962449,-29.6653417898471)) ;
#8602 = CARTESIAN_POINT('Ctrl Pts',(-10.5823802426207,3.09180943533062,-29.6653338028838)) ;
#8603 = CARTESIAN_POINT('Ctrl Pts',(-10.5824983793995,3.10764226162414,-29.6651022683863)) ;
#8604 = CARTESIAN_POINT('Ctrl Pts',(-10.5816487421359,3.12340351212708,-29.6636948191982)) ;
#8605 = CARTESIAN_POINT('Ctrl Pts',(-10.5798917143156,3.13890174174782,-29.661194637388)) ;
#8606 = CARTESIAN_POINT('Ctrl Pts',(-10.5788154289346,3.14839534098403,-29.6596631254215)) ;
#8607 = CARTESIAN_POINT('Ctrl Pts',(-10.5773980105714,3.15779035973712,-29.6577207127312)) ;
#8608 = CARTESIAN_POINT('Ctrl Pts',(-10.575648075692,3.16704107189944,-29.6553786680892)) ;
#8609 = CARTESIAN_POINT('Ctrl Pts',(-10.572793572054,3.18213088571561,-29.6515583116694)) ;
#8610 = CARTESIAN_POINT('Ctrl Pts',(-10.5690737974298,3.1967412659164,-29.6467011743094)) ;
#8611 = CARTESIAN_POINT('Ctrl Pts',(-10.5645335593023,3.21067545103312,-29.6408676243673)) ;
#8612 = CARTESIAN_POINT('Ctrl Pts',(-10.5617972837458,3.21907319781733,-29.6373519056613)) ;
#8613 = CARTESIAN_POINT('Ctrl Pts',(-10.5587624736304,3.22722513283465,-29.6334807311337)) ;
#8614 = CARTESIAN_POINT('Ctrl Pts',(-10.5554349224176,3.23508368100507,-29.6292603598437)) ;
#8615 = CARTESIAN_POINT('Ctrl Pts',(-10.5529664611125,3.24091334998174,-29.6261295821166)) ;
#8616 = CARTESIAN_POINT('Ctrl Pts',(-10.5503452912355,3.24656143395102,-29.6228172996488)) ;
#8617 = CARTESIAN_POINT('Ctrl Pts',(-10.5475756406467,3.25201040996413,-29.6193284766451)) ;
#8618 = CARTESIAN_POINT('Ctrl Pts',(-10.541406136158,3.26414821612172,-29.6115569876104)) ;
#8619 = CARTESIAN_POINT('Ctrl Pts',(-10.5345010451408,3.27530068412359,-29.6029117174434)) ;
#8620 = CARTESIAN_POINT('Ctrl Pts',(-10.5269668631543,3.28536494341284,-29.5935395852846)) ;
#8621 = CARTESIAN_POINT('Ctrl Pts',(-10.5222573308481,3.29165599854599,-29.5876811710256)) ;
#8622 = CARTESIAN_POINT('Ctrl Pts',(-10.5173015595218,3.29752119279001,-29.5815380059231)) ;
#8623 = CARTESIAN_POINT('Ctrl Pts',(-10.5121231599117,3.30292691930815,-29.5751405663713)) ;
#8624 = CARTESIAN_POINT('Ctrl Pts',(-10.5036737279875,3.31174727340488,-29.5647020652798)) ;
#8625 = CARTESIAN_POINT('Ctrl Pts',(-10.494711970624,3.31926224841926,-29.5536886810406)) ;
#8626 = CARTESIAN_POINT('Ctrl Pts',(-10.4853613533682,3.32535947250976,-29.5422471616422)) ;
#8627 = CARTESIAN_POINT('Ctrl Pts',(-10.4760107361123,3.33145669660025,-29.5308056422437)) ;
#8628 = CARTESIAN_POINT('Ctrl Pts',(-10.4662702167324,3.33613714779707,-29.5189348436387)) ;
#8629 = CARTESIAN_POINT('Ctrl Pts',(-10.4562560925639,3.33923511979837,-29.5067623750852)) ;
#8630 = CARTESIAN_POINT('Origin',(1.11022302462516E-15,3.05,-16.8941925465839)) ;
#8631 = CARTESIAN_POINT('',(9.98909940046138,3.3,-29.82)) ;
#8632 = CARTESIAN_POINT('',(10.1419706226055,3.05,-30.01781402741)) ;
#8633 = CARTESIAN_POINT('Origin',(9.98909940046138,3.05,-29.82)) ;
#8634 = CARTESIAN_POINT('Origin',(1.11022302462516E-15,3.05,-16.8941925465839)) ;
#8635 = CARTESIAN_POINT('Origin',(1.11022302462516E-15,3.3,-16.8941925465839)) ;
#8636 = CARTESIAN_POINT('Ctrl Pts',(9.98909940046138,3.3,-29.82)) ;
#8637 = CARTESIAN_POINT('Ctrl Pts',(10.147749113045,3.3,-29.7175603525465)) ;
#8638 = CARTESIAN_POINT('Ctrl Pts',(10.3042079931798,3.3122986306003,-29.6126005064717)) ;
#8639 = CARTESIAN_POINT('Ctrl Pts',(10.4562560925639,3.33923511979837,-29.5067623750852)) ;
#8640 = CARTESIAN_POINT('Ctrl Pts',(10.0291209928308,3.3,-29.871787591274)) ;
#8641 = CARTESIAN_POINT('Ctrl Pts',(10.1867667904972,3.29572909993472,-29.7667751370844)) ;
#8642 = CARTESIAN_POINT('Ctrl Pts',(10.3424189419942,3.30453465713751,-29.6585580134996)) ;
#8643 = CARTESIAN_POINT('Ctrl Pts',(10.4937439232518,3.32847961370676,-29.5490226213438)) ;
#8644 = CARTESIAN_POINT('Ctrl Pts',(10.1087705983176,3.24570589574959,-29.9748534857044)) ;
#8645 = CARTESIAN_POINT('Ctrl Pts',(10.2645399752038,3.23788937883,-29.8603708829999)) ;
#8646 = CARTESIAN_POINT('Ctrl Pts',(10.4185497613911,3.24402514762919,-29.742418677397)) ;
#8647 = CARTESIAN_POINT('Ctrl Pts',(10.5685054554551,3.2669079755233,-29.62309040069)) ;
#8648 = CARTESIAN_POINT('Ctrl Pts',(10.1419706226055,3.11544984694979,-30.01781402741)) ;
#8649 = CARTESIAN_POINT('Ctrl Pts',(10.3004417599092,3.11276689086104,-29.895237357648)) ;
#8650 = CARTESIAN_POINT('Ctrl Pts',(10.4570254125938,3.12464176082151,-29.7697804551426)) ;
#8651 = CARTESIAN_POINT('Ctrl Pts',(10.6091727180391,3.15371643721036,-29.6430963665886)) ;
#8652 = CARTESIAN_POINT('Ctrl Pts',(10.1419706226055,3.05,-30.01781402741)) ;
#8653 = CARTESIAN_POINT('Ctrl Pts',(10.3030482793393,3.05,-29.8933327731359)) ;
#8654 = CARTESIAN_POINT('Ctrl Pts',(10.4619015755534,3.06471962087595,-29.7657890572739)) ;
#8655 = CARTESIAN_POINT('Ctrl Pts',(10.6162765892914,3.09695856857757,-29.6371780782973)) ;
#8656 = CARTESIAN_POINT('Ctrl Pts',(10.582363125788,3.09017060002378,-29.6653547280519)) ;
#8657 = CARTESIAN_POINT('Ctrl Pts',(10.4386734667128,3.06264696571336,-29.7844130751078)) ;
#8658 = CARTESIAN_POINT('Ctrl Pts',(10.2912776199237,3.05,-29.902429170969)) ;
#8659 = CARTESIAN_POINT('Ctrl Pts',(10.1419706226055,3.05,-30.01781402741)) ;
#8660 = CARTESIAN_POINT('Ctrl Pts',(9.98909940046138,3.3,-29.82)) ;
#8661 = CARTESIAN_POINT('Ctrl Pts',(10.147749113045,3.3,-29.7175603525465)) ;
#8662 = CARTESIAN_POINT('Ctrl Pts',(10.3042079931798,3.3122986306003,-29.6126005064717)) ;
#8663 = CARTESIAN_POINT('Ctrl Pts',(10.4562560925639,3.33923511979837,-29.5067623750852)) ;
#8664 = CARTESIAN_POINT('Origin',(1.11022302462516E-15,3.05,-16.8941925465839)) ;
#8665 = CARTESIAN_POINT('',(-10.9348219720805,3.05,-29.3649053297691)) ;
#8666 = CARTESIAN_POINT('Origin',(-10.77,3.05,-29.176932678781)) ;
#8667 = CARTESIAN_POINT('Origin',(1.11022302462516E-15,3.05,-16.8941925465839)) ;
#8668 = CARTESIAN_POINT('Ctrl Pts',(-10.77,3.3,-29.176932678781)) ;
#8669 = CARTESIAN_POINT('Ctrl Pts',(-10.6644750033044,3.3,-29.2876755180678)) ;
#8670 = CARTESIAN_POINT('Ctrl Pts',(-10.5574497695917,3.31311478519588,-29.3965002427796)) ;
#8671 = CARTESIAN_POINT('Ctrl Pts',(-10.4512438343541,3.34065281272427,-29.501243923759)) ;
#8672 = CARTESIAN_POINT('Ctrl Pts',(-10.8131502913865,3.3,-29.2261438037327)) ;
#8673 = CARTESIAN_POINT('Ctrl Pts',(-10.7056436255395,3.29633423430578,-29.3355995974397)) ;
#8674 = CARTESIAN_POINT('Ctrl Pts',(-10.5959487962567,3.30645872447267,-29.4433768078905)) ;
#8675 = CARTESIAN_POINT('Ctrl Pts',(-10.4867185411393,3.33145461255,-29.5471888940564)) ;
#8676 = CARTESIAN_POINT('Ctrl Pts',(-10.8990265225851,3.24570588944608,-29.3240820981936)) ;
#8677 = CARTESIAN_POINT('Ctrl Pts',(-10.7830438290636,3.2389968774968,-29.4311063020667)) ;
#8678 = CARTESIAN_POINT('Ctrl Pts',(-10.6646000202357,3.24691483243654,-29.5367571598192)) ;
#8679 = CARTESIAN_POINT('Ctrl Pts',(-10.5465724667282,3.27117973026827,-29.6387913916651)) ;
#8680 = CARTESIAN_POINT('Ctrl Pts',(-10.9348219720805,3.11544984694979,-29.3649053297691)) ;
#8681 = CARTESIAN_POINT('Ctrl Pts',(-10.8096178153564,3.11314703296704,-29.474590241034)) ;
#8682 = CARTESIAN_POINT('Ctrl Pts',(-10.6826104679429,3.12626473336083,-29.5827439357331)) ;
#8683 = CARTESIAN_POINT('Ctrl Pts',(-10.5563795789494,3.15628364564047,-29.6868463778552)) ;
#8684 = CARTESIAN_POINT('Ctrl Pts',(-10.9348219720805,3.05,-29.3649053297691)) ;
#8685 = CARTESIAN_POINT('Ctrl Pts',(-10.8065915039709,3.05,-29.4773429557936)) ;
#8686 = CARTESIAN_POINT('Ctrl Pts',(-10.6765379977093,3.06569643582498,-29.587833112793)) ;
#8687 = CARTESIAN_POINT('Ctrl Pts',(-10.5474800757194,3.09865533491409,-29.6941797705656)) ;
#8688 = CARTESIAN_POINT('Ctrl Pts',(-10.5823626153175,3.09017135645643,-29.6653548535384)) ;
#8689 = CARTESIAN_POINT('Ctrl Pts',(-10.6999427554713,3.06299713058314,-29.5679206810131)) ;
#8690 = CARTESIAN_POINT('Ctrl Pts',(-10.8181371295452,3.05,-29.4672192874512)) ;
#8691 = CARTESIAN_POINT('Ctrl Pts',(-10.9348219720805,3.05,-29.3649053297691)) ;
#8692 = CARTESIAN_POINT('',(-10.4512438329193,3.34065280720824,-29.5012439237535)) ;
#8693 = CARTESIAN_POINT('Ctrl Pts',(-10.77,3.3,-29.176932678781)) ;
#8694 = CARTESIAN_POINT('Ctrl Pts',(-10.6644750033044,3.3,-29.2876755180678)) ;
#8695 = CARTESIAN_POINT('Ctrl Pts',(-10.5574497695917,3.31311478519588,-29.3965002427796)) ;
#8696 = CARTESIAN_POINT('Ctrl Pts',(-10.4512438343541,3.34065281272427,-29.501243923759)) ;
#8697 = CARTESIAN_POINT('Ctrl Pts',(-10.4512438793665,3.34065280105307,-29.5012438793665)) ;
#8698 = CARTESIAN_POINT('Ctrl Pts',(-10.4530174819393,3.34019292553853,-29.5030174819393)) ;
#8699 = CARTESIAN_POINT('Ctrl Pts',(-10.4546884899342,3.33972007374684,-29.504856907029)) ;
#8700 = CARTESIAN_POINT('Ctrl Pts',(-10.4562560925639,3.33923511979837,-29.5067623750852)) ;
#8701 = CARTESIAN_POINT('Origin',(1.11022302462516E-15,3.05,-16.8941925465839)) ;
#8702 = CARTESIAN_POINT('',(11.7,3.05,-28.65)) ;
#8703 = CARTESIAN_POINT('Origin',(1.11022302462516E-15,3.05,-16.8941925465839)) ;
#8704 = CARTESIAN_POINT('Ctrl Pts',(11.5234344017195,3.3,-28.4730122076873)) ;
#8705 = CARTESIAN_POINT('Ctrl Pts',(11.5248174913711,3.3,-28.4743986171276)) ;
#8706 = CARTESIAN_POINT('Ctrl Pts',(11.5262005335001,3.29997698962269,-28.4757849786486)) ;
#8707 = CARTESIAN_POINT('Ctrl Pts',(11.5499521209721,3.29918654602495,-28.4995935660222)) ;
#8708 = CARTESIAN_POINT('Ctrl Pts',(11.5720185826081,3.29242837601996,-28.5217129029717)) ;
#8709 = CARTESIAN_POINT('Ctrl Pts',(11.6137589203932,3.26726387117987,-28.5635531294919)) ;
#8710 = CARTESIAN_POINT('Ctrl Pts',(11.6329511205595,3.24878239907886,-28.582791187992)) ;
#8711 = CARTESIAN_POINT('Ctrl Pts',(11.6652519474717,3.20244341327706,-28.6151691262907)) ;
#8712 = CARTESIAN_POINT('Ctrl Pts',(11.6780517643177,3.17502893211499,-28.62799946099)) ;
#8713 = CARTESIAN_POINT('Ctrl Pts',(11.6955092411613,3.11479613681801,-28.6454985466269)) ;
#8714 = CARTESIAN_POINT('Ctrl Pts',(11.7,3.08255368454763,-28.65)) ;
#8715 = CARTESIAN_POINT('Ctrl Pts',(11.7,3.05,-28.65)) ;
#8716 = CARTESIAN_POINT('Origin',(21.8132129304798,3.05,-18.1832336789269)) ;
#8717 = CARTESIAN_POINT('',(21.9899896257764,3.05,-18.3600103742236)) ;
#8718 = CARTESIAN_POINT('Origin',(-24.5,3.05,-7.145)) ;
#8719 = CARTESIAN_POINT('',(-24.75,3.05,33.25)) ;
#8720 = CARTESIAN_POINT('',(-24.75,3.05,-7.145)) ;
#8721 = CARTESIAN_POINT('Origin',(-24.5,3.05,33.25)) ;
#8722 = CARTESIAN_POINT('Origin',(24.5,3.05,16.63)) ;
#8723 = CARTESIAN_POINT('',(24.75,3.05,33.25)) ;
#8724 = CARTESIAN_POINT('Origin',(24.5,3.05,33.25)) ;
#8725 = CARTESIAN_POINT('',(24.75,3.05,16.63)) ;
#8726 = CARTESIAN_POINT('Origin',(-12.2500207484472,3.05,33.25)) ;
#8727 = CARTESIAN_POINT('',(-24.5,3.05,33.5)) ;
#8728 = CARTESIAN_POINT('Origin',(-24.5,3.05,33.25)) ;
#8729 = CARTESIAN_POINT('',(-10.77,3.05,33.5)) ;
#8730 = CARTESIAN_POINT('',(-12.2500207484472,3.05,33.5)) ;
#8731 = CARTESIAN_POINT('Origin',(-10.77,3.05,33.25)) ;
#8732 = CARTESIAN_POINT('Origin',(-10.77,4.57,33.25)) ;
#8733 = CARTESIAN_POINT('',(-9.25,4.57,33.5)) ;
#8734 = CARTESIAN_POINT('',(-9.5,4.57,33.25)) ;
#8735 = CARTESIAN_POINT('Origin',(-9.25,4.57,33.25)) ;
#8736 = CARTESIAN_POINT('Origin',(-10.77,4.57,33.25)) ;
#8737 = CARTESIAN_POINT('Origin',(-10.77,4.57,33.5)) ;
#8738 = CARTESIAN_POINT('Origin',(-9.25,8.6875,33.25)) ;
#8739 = CARTESIAN_POINT('',(-9.25,24.6003192917499,33.5)) ;
#8740 = CARTESIAN_POINT('',(-9.5,24.6003192917499,33.25)) ;
#8741 = CARTESIAN_POINT('Origin',(-9.25,24.6003192917499,33.25)) ;
#8742 = CARTESIAN_POINT('',(-9.5,8.6875,33.25)) ;
#8743 = CARTESIAN_POINT('',(-9.25,8.6875,33.5)) ;
#8744 = CARTESIAN_POINT('Ctrl Pts',(-9.25,24.6003192917499,33.5)) ;
#8745 = CARTESIAN_POINT('Ctrl Pts',(-9.25,25.370369005669,33.5)) ;
#8746 = CARTESIAN_POINT('Ctrl Pts',(-8.81719996776914,27.1694431484448,33.5)) ;
#8747 = CARTESIAN_POINT('Ctrl Pts',(-7.54929504861548,28.2003141923527,33.5)) ;
#8748 = CARTESIAN_POINT('Ctrl Pts',(-6.76795090667124,28.3557987366091,33.5)) ;
#8749 = CARTESIAN_POINT('Ctrl Pts',(-9.31544984694979,24.6003192917499,33.5)) ;
#8750 = CARTESIAN_POINT('Ctrl Pts',(-9.31001237129096,25.3805985297588,33.4998240176448)) ;
#8751 = CARTESIAN_POINT('Ctrl Pts',(-8.85942127194599,27.1975612821968,33.4998356946794)) ;
#8752 = CARTESIAN_POINT('Ctrl Pts',(-7.56933624934574,28.2354900210942,33.5000078650668)) ;
#8753 = CARTESIAN_POINT('Ctrl Pts',(-6.77517359820447,28.3920943552222,33.5)) ;
#8754 = CARTESIAN_POINT('Ctrl Pts',(-9.44567143792189,24.6003192917499,33.4456714379219)) ;
#8755 = CARTESIAN_POINT('Ctrl Pts',(-9.4298299112322,25.4008861366219,33.4551270066274)) ;
#8756 = CARTESIAN_POINT('Ctrl Pts',(-8.94398652948135,27.2537008535442,33.4736901555626)) ;
#8757 = CARTESIAN_POINT('Ctrl Pts',(-7.60938939076493,28.3057987139221,33.4819757476224)) ;
#8758 = CARTESIAN_POINT('Ctrl Pts',(-6.789611851291,28.464649762726,33.483268532741)) ;
#8759 = CARTESIAN_POINT('Ctrl Pts',(-9.5,24.6003192917499,33.3154498469498)) ;
#8760 = CARTESIAN_POINT('Ctrl Pts',(-9.49134428057035,25.4094606950313,33.342417324315)) ;
#8761 = CARTESIAN_POINT('Ctrl Pts',(-9.00760901658298,27.2899950446831,33.4011943379152)) ;
#8762 = CARTESIAN_POINT('Ctrl Pts',(-7.64149663567344,28.3614500536775,33.4317712233585)) ;
#8763 = CARTESIAN_POINT('Ctrl Pts',(-6.80125367349474,28.5231524880223,33.4364220663262)) ;
#8764 = CARTESIAN_POINT('Ctrl Pts',(-9.5,24.6003192917499,33.25)) ;
#8765 = CARTESIAN_POINT('Ctrl Pts',(-9.5,25.4093792116268,33.2823374075703)) ;
#8766 = CARTESIAN_POINT('Ctrl Pts',(-9.03020851202291,27.2995932530022,33.3578875866726)) ;
#8767 = CARTESIAN_POINT('Ctrl Pts',(-7.65393565106124,28.3826875378412,33.4011779048128)) ;
#8768 = CARTESIAN_POINT('Ctrl Pts',(-6.80580995852349,28.5460488256182,33.407707310626)) ;
#8769 = CARTESIAN_POINT('',(-7.77490213744258,27.9,33.5)) ;
#8770 = CARTESIAN_POINT('',(-6.80580995852373,28.5460488256181,33.407707310626)) ;
#8771 = CARTESIAN_POINT('Ctrl Pts',(-7.77490213744258,27.9,33.5)) ;
#8772 = CARTESIAN_POINT('Ctrl Pts',(-7.78114603380676,27.9,33.5)) ;
#8773 = CARTESIAN_POINT('Ctrl Pts',(-7.78788956564949,27.9005807447427,33.4999170364653)) ;
#8774 = CARTESIAN_POINT('Ctrl Pts',(-7.79738323625925,27.9036098316155,33.4994843097692)) ;
#8775 = CARTESIAN_POINT('Ctrl Pts',(-7.80075984355882,27.9052369392644,33.4992518658196)) ;
#8776 = CARTESIAN_POINT('Ctrl Pts',(-7.8058478238372,27.9094255221287,33.498653496839)) ;
#8777 = CARTESIAN_POINT('Ctrl Pts',(-7.80764775880098,27.9116123995803,33.4983410857742)) ;
#8778 = CARTESIAN_POINT('Ctrl Pts',(-7.81039359400954,27.9168212609468,33.4975969627219)) ;
#8779 = CARTESIAN_POINT('Ctrl Pts',(-7.81121069749947,27.9197085232834,33.4971844966738)) ;
#8780 = CARTESIAN_POINT('Ctrl Pts',(-7.81218916899328,27.927178867045,33.4961173047079)) ;
#8781 = CARTESIAN_POINT('Ctrl Pts',(-7.81180402710554,27.9318932870624,33.4954438161339)) ;
#8782 = CARTESIAN_POINT('Ctrl Pts',(-7.80918949730732,27.9458600663565,33.4934485619491)) ;
#8783 = CARTESIAN_POINT('Ctrl Pts',(-7.80504750550433,27.9558650275853,33.4920192817735)) ;
#8784 = CARTESIAN_POINT('Ctrl Pts',(-7.78977167890809,27.9863923872478,33.4876582303932)) ;
#8785 = CARTESIAN_POINT('Ctrl Pts',(-7.77102732566492,28.0128597160257,33.483877183425)) ;
#8786 = CARTESIAN_POINT('Ctrl Pts',(-7.68861250822215,28.1074719134625,33.4703611552197)) ;
#8787 = CARTESIAN_POINT('Ctrl Pts',(-7.59512622632696,28.1900482534497,33.4585645351902)) ;
#8788 = CARTESIAN_POINT('Ctrl Pts',(-7.29573476020478,28.3831508397044,33.4309784514395)) ;
#8789 = CARTESIAN_POINT('Ctrl Pts',(-7.07088849616787,28.486213422642,33.4162552253368)) ;
#8790 = CARTESIAN_POINT('Ctrl Pts',(-6.80580995852349,28.5460488256182,33.407707310626)) ;
#8791 = CARTESIAN_POINT('Origin',(-6.325,24.6003192917499,33.25)) ;
#8792 = CARTESIAN_POINT('Origin',(-6.325,24.6003192917499,33.5)) ;
#8793 = CARTESIAN_POINT('Origin',(-24.5,3.05,33.25)) ;
#8794 = CARTESIAN_POINT('Origin',(-24.5,3.05,33.25)) ;
#8795 = CARTESIAN_POINT('Origin',(24.5,3.05,33.25)) ;
#8796 = CARTESIAN_POINT('Origin',(24.5,3.05,33.25)) ;
#8797 = CARTESIAN_POINT('Origin',(9.5,17.375,2.475)) ;
#8798 = CARTESIAN_POINT('',(9.5,4.57,-28.55)) ;
#8799 = CARTESIAN_POINT('',(9.5,4.57,1.2425)) ;
#8800 = CARTESIAN_POINT('',(9.5,12.6602026834209,-28.55)) ;
#8801 = CARTESIAN_POINT('',(9.5,3.,-28.55)) ;
#8802 = CARTESIAN_POINT('',(9.5,28.157290298199,23.106958715927)) ;
#8803 = CARTESIAN_POINT('',(9.5,17.5986951224045,-12.0883585367213)) ;
#8804 = CARTESIAN_POINT('',(9.5,28.5749851188244,25.8674171460039)) ;
#8805 = CARTESIAN_POINT('Origin',(9.5,18.3909804312853,25.996564592546)) ;
#8806 = CARTESIAN_POINT('',(9.5,28.575,14.1625)) ;
#8807 = CARTESIAN_POINT('Origin',(10.77,4.57,1.2425)) ;
#8808 = CARTESIAN_POINT('Origin',(10.77,4.57,-29.82)) ;
#8809 = CARTESIAN_POINT('Origin',(-4.14968943118765E-5,3.3,0.0099999999999989)) ;
#8810 = CARTESIAN_POINT('',(-4.75002074844716,3.3,-29.82)) ;
#8811 = CARTESIAN_POINT('Origin',(-4.75002074844716,4.57,-29.82)) ;
#8812 = CARTESIAN_POINT('',(-9.5,4.57,-28.55)) ;
#8813 = CARTESIAN_POINT('Origin',(-10.77,4.57,-29.82)) ;
#8814 = CARTESIAN_POINT('',(-4.75002074844716,4.57,-28.55)) ;
#8815 = CARTESIAN_POINT('Origin',(-10.77,4.57,1.2425)) ;
#8816 = CARTESIAN_POINT('',(-9.5,4.57,1.2425)) ;
#8817 = CARTESIAN_POINT('Origin',(-9.5,17.375,2.475)) ;
#8818 = CARTESIAN_POINT('',(-9.5,28.575,28.455147082111)) ;
#8819 = CARTESIAN_POINT('',(-9.5,33.0419144924728,23.0664883292866)) ;
#8820 = CARTESIAN_POINT('',(-9.5,28.575,25.8674157457972)) ;
#8821 = CARTESIAN_POINT('',(-9.5,28.575,14.1625)) ;
#8822 = CARTESIAN_POINT('',(-9.5,28.1572902981989,23.1069587159267)) ;
#8823 = CARTESIAN_POINT('Origin',(-9.5,18.3909804312853,25.996564592546)) ;
#8824 = CARTESIAN_POINT('',(-9.5,12.6602026834209,-28.55)) ;
#8825 = CARTESIAN_POINT('',(-9.5,17.5986951224045,-12.0883585367213)) ;
#8826 = CARTESIAN_POINT('',(-9.5,3.,-28.55)) ;
#8827 = CARTESIAN_POINT('Origin',(-6.325,33.0419144924728,23.0664883292866)) ;
#8828 = CARTESIAN_POINT('Origin',(-6.325,28.575,28.455147082111)) ;
#8829 = CARTESIAN_POINT('Origin',(-6.325,23.9220039727312,34.0682851467527)) ;
#8830 = CARTESIAN_POINT('Origin',(6.325,18.3909804312853,25.996564592546)) ;
#8831 = CARTESIAN_POINT('',(6.325,31.2,22.2)) ;
#8832 = CARTESIAN_POINT('',(6.325,31.75,25.85)) ;
#8833 = CARTESIAN_POINT('Origin',(6.325,18.3909804312853,25.996564592546)) ;
#8834 = CARTESIAN_POINT('Ctrl Pts',(6.325,31.75,25.85)) ;
#8835 = CARTESIAN_POINT('Ctrl Pts',(6.43046220354674,31.74999470036,25.8495169502164)) ;
#8836 = CARTESIAN_POINT('Ctrl Pts',(6.53592423385766,31.7447307283387,25.8490915953681)) ;
#8837 = CARTESIAN_POINT('Ctrl Pts',(6.64086325133653,31.7342341731504,25.8487253551069)) ;
#8838 = CARTESIAN_POINT('Ctrl Pts',(6.74579915993031,31.7237379289293,25.8483591256958)) ;
#8839 = CARTESIAN_POINT('Ctrl Pts',(6.85021174198924,31.7080094463137,25.8480520088604)) ;
#8840 = CARTESIAN_POINT('Ctrl Pts',(6.95358339129659,31.6871266888496,25.847804826769)) ;
#8841 = CARTESIAN_POINT('Ctrl Pts',(7.05695217787227,31.666244509704,25.847557651523)) ;
#8842 = CARTESIAN_POINT('Ctrl Pts',(7.15927974986701,31.6402084100166,25.847370408779)) ;
#8843 = CARTESIAN_POINT('Ctrl Pts',(7.260058865173,31.6091474441695,25.8472433040211)) ;
#8844 = CARTESIAN_POINT('Ctrl Pts',(7.3608353843029,31.5780872784856,25.8471162025376)) ;
#8845 = CARTESIAN_POINT('Ctrl Pts',(7.4600631956079,31.5420026077587,25.847049236588)) ;
#8846 = CARTESIAN_POINT('Ctrl Pts',(7.55725044792966,31.5010722880811,25.8470419821051)) ;
#8847 = CARTESIAN_POINT('Ctrl Pts',(7.6544353845022,31.460142943679,25.8470347277951)) ;
#8848 = CARTESIAN_POINT('Ctrl Pts',(7.74957954026074,31.4143683158502,25.8470871823076)) ;
#8849 = CARTESIAN_POINT('Ctrl Pts',(7.84221132830012,31.363975280532,25.847198285725)) ;
#8850 = CARTESIAN_POINT('Ctrl Pts',(7.934841088328,31.3135833484815,25.8473093867099)) ;
#8851 = CARTESIAN_POINT('Ctrl Pts',(8.0249582865672,31.2585733768047,25.8474791337795)) ;
#8852 = CARTESIAN_POINT('Ctrl Pts',(8.1121162720151,31.199218004425,25.8477058315995)) ;
#8853 = CARTESIAN_POINT('Ctrl Pts',(8.19927251801032,31.1398638166283,25.8479325248951)) ;
#8854 = CARTESIAN_POINT('Ctrl Pts',(8.28346938325736,31.0761645966036,25.8482161659582)) ;
#8855 = CARTESIAN_POINT('Ctrl Pts',(8.36428957653771,31.0084360368315,25.8485544313)) ;
#8856 = CARTESIAN_POINT('Ctrl Pts',(8.44510831342536,30.9407086975387,25.8488926905462)) ;
#8857 = CARTESIAN_POINT('Ctrl Pts',(8.52255023480056,30.8689523861978,25.8492855709361)) ;
#8858 = CARTESIAN_POINT('Ctrl Pts',(8.59623154168566,30.7935227137269,25.8497301349389)) ;
#8859 = CARTESIAN_POINT('Ctrl Pts',(8.66992458575925,30.7180810255587,25.8501747697592)) ;
#8860 = CARTESIAN_POINT('Ctrl Pts',(8.73985557411532,30.6389650526736,25.8506711030591)) ;
#8861 = CARTESIAN_POINT('Ctrl Pts',(8.80567782139028,30.5565670039655,25.8512156022673)) ;
#8862 = CARTESIAN_POINT('Ctrl Pts',(8.87149635540453,30.4741736036164,25.8517600707585)) ;
#8863 = CARTESIAN_POINT('Ctrl Pts',(8.9332063960891,30.388498768684,25.8523526976616)) ;
#8864 = CARTESIAN_POINT('Ctrl Pts',(8.99050204818587,30.2999671749436,25.8529893849969)) ;
#8865 = CARTESIAN_POINT('Ctrl Pts',(9.04779491311263,30.2114398878581,25.8536260413604)) ;
#8866 = CARTESIAN_POINT('Ctrl Pts',(9.10067363112342,30.1200564108484,25.8543067513843)) ;
#8867 = CARTESIAN_POINT('Ctrl Pts',(9.1488761090875,30.0262696721175,25.8550268858408)) ;
#8868 = CARTESIAN_POINT('Ctrl Pts',(9.19707661659256,29.9324867672751,25.8557469908591)) ;
#8869 = CARTESIAN_POINT('Ctrl Pts',(9.2406011084124,29.8363011052836,25.8565065141989)) ;
#8870 = CARTESIAN_POINT('Ctrl Pts',(9.27923387320771,29.7381893761549,25.8573003357022)) ;
#8871 = CARTESIAN_POINT('Ctrl Pts',(9.317871729721,29.6400647161046,25.8580942618295)) ;
#8872 = CARTESIAN_POINT('Ctrl Pts',(9.35161644172219,29.5400138030315,25.8589224919069)) ;
#8873 = CARTESIAN_POINT('Ctrl Pts',(9.38030072332849,29.4385326126193,25.8597794581924)) ;
#8874 = CARTESIAN_POINT('Ctrl Pts',(9.40898209837118,29.3370617052442,25.860636337642)) ;
#8875 = CARTESIAN_POINT('Ctrl Pts',(9.43260397516068,29.234161143853,25.8615219438564)) ;
#8876 = CARTESIAN_POINT('Ctrl Pts',(9.4510492744072,29.1303409262827,25.8624303169636)) ;
#8877 = CARTESIAN_POINT('Ctrl Pts',(9.4694959506141,29.0265129584274,25.8633387578817)) ;
#8878 = CARTESIAN_POINT('Ctrl Pts',(9.48276521515409,28.921765537959,25.8642699651669)) ;
#8879 = CARTESIAN_POINT('Ctrl Pts',(9.49079129054069,28.8166178923319,25.8652176403169)) ;
#8880 = CARTESIAN_POINT('Ctrl Pts',(9.49692746081675,28.7362294301487,25.8659421657925)) ;
#8881 = CARTESIAN_POINT('Ctrl Pts',(9.5,28.6556072605121,25.8666763094571)) ;
#8882 = CARTESIAN_POINT('Ctrl Pts',(9.5,28.5749851188244,25.8674171460039)) ;
#8883 = CARTESIAN_POINT('Ctrl Pts',(9.5,28.157290298199,23.106958715927)) ;
#8884 = CARTESIAN_POINT('Ctrl Pts',(9.5,28.1804450776003,23.1000600670451)) ;
#8885 = CARTESIAN_POINT('Ctrl Pts',(9.49972422059564,28.203599079594,23.0931615647751)) ;
#8886 = CARTESIAN_POINT('Ctrl Pts',(9.4985130472546,28.2544365009203,23.0780148814088)) ;
#8887 = CARTESIAN_POINT('Ctrl Pts',(9.49745895112732,28.2821152676473,23.0697680502854)) ;
#8888 = CARTESIAN_POINT('Ctrl Pts',(9.49333672763788,28.3608494434134,23.0463090288973)) ;
#8889 = CARTESIAN_POINT('Ctrl Pts',(9.48931972873393,28.4118497186112,23.031112980272)) ;
#8890 = CARTESIAN_POINT('Ctrl Pts',(9.47326463912736,28.5643586303592,22.985670233064)) ;
#8891 = CARTESIAN_POINT('Ctrl Pts',(9.45723262679727,28.6654075247228,22.9555593489331)) ;
#8892 = CARTESIAN_POINT('Ctrl Pts',(9.39330812722704,28.965714961593,22.8660684272176)) ;
#8893 = CARTESIAN_POINT('Ctrl Pts',(9.32974954840376,29.1613140148577,22.8077745275644)) ;
#8894 = CARTESIAN_POINT('Ctrl Pts',(9.08425034832404,29.7138633169295,22.64308623758)) ;
#8895 = CARTESIAN_POINT('Ctrl Pts',(8.84953554453401,30.0445944579936,22.5444934762977)) ;
#8896 = CARTESIAN_POINT('Ctrl Pts',(8.26103034811584,30.6012160783936,22.3785462415353)) ;
#8897 = CARTESIAN_POINT('Ctrl Pts',(7.91286656009489,30.8217851943026,22.3127786094015)) ;
#8898 = CARTESIAN_POINT('Ctrl Pts',(7.14791041241991,31.1226151396577,22.2230766109168)) ;
#8899 = CARTESIAN_POINT('Ctrl Pts',(6.73843153640591,31.2000000000001,22.2000000000002)) ;
#8900 = CARTESIAN_POINT('Ctrl Pts',(6.325,31.2000000000001,22.2000000000003)) ;
#8901 = CARTESIAN_POINT('Origin',(6.325,28.575,14.1625)) ;
#8902 = CARTESIAN_POINT('',(6.325,31.75,14.1625)) ;
#8903 = CARTESIAN_POINT('Origin',(6.325,17.5986951224045,-12.0883585367213)) ;
#8904 = CARTESIAN_POINT('',(9.36972204690191,13.6,-28.55)) ;
#8905 = CARTESIAN_POINT('Origin',(6.325,12.6602026834209,-28.55)) ;
#8906 = CARTESIAN_POINT('',(6.325,16.65,-26.3)) ;
#8907 = CARTESIAN_POINT('Ctrl Pts',(9.36972204690191,13.6,-28.55)) ;
#8908 = CARTESIAN_POINT('Ctrl Pts',(9.33150428640196,13.7352848730332,-28.5489172081766)) ;
#8909 = CARTESIAN_POINT('Ctrl Pts',(9.28537554981067,13.8692960232194,-28.5392936237713)) ;
#8910 = CARTESIAN_POINT('Ctrl Pts',(9.06189751586222,14.4233292907506,-28.4655098589506)) ;
#8911 = CARTESIAN_POINT('Ctrl Pts',(8.81830342317927,14.8140076105995,-28.324179740912)) ;
#8912 = CARTESIAN_POINT('Ctrl Pts',(8.20202480438423,15.5807535317409,-27.9023312808353)) ;
#8913 = CARTESIAN_POINT('Ctrl Pts',(7.77008447929203,15.9418765716257,-27.5554690453292)) ;
#8914 = CARTESIAN_POINT('Ctrl Pts',(7.18160415304357,16.3103729693986,-27.046927007198)) ;
#8915 = CARTESIAN_POINT('Ctrl Pts',(6.98513622894908,16.4114752355335,-26.8706894533264)) ;
#8916 = CARTESIAN_POINT('Ctrl Pts',(6.7262959895539,16.524579645383,-26.6336670195021)) ;
#8917 = CARTESIAN_POINT('Ctrl Pts',(6.64224012239147,16.5576770884375,-26.5557152165318)) ;
#8918 = CARTESIAN_POINT('Ctrl Pts',(6.52704506600961,16.5986811618034,-26.4494819237855)) ;
#8919 = CARTESIAN_POINT('Ctrl Pts',(6.48975900833928,16.611175247101,-26.4152486293163)) ;
#8920 = CARTESIAN_POINT('Ctrl Pts',(6.43498907397076,16.6280885098712,-26.3665958960957)) ;
#8921 = CARTESIAN_POINT('Ctrl Pts',(6.41711081442205,16.6333341653242,-26.3511046831613)) ;
#8922 = CARTESIAN_POINT('Ctrl Pts',(6.38827974448016,16.6407770204755,-26.3285991010218)) ;
#8923 = CARTESIAN_POINT('Ctrl Pts',(6.37860103000991,16.6431409047043,-26.3213573070103)) ;
#8924 = CARTESIAN_POINT('Ctrl Pts',(6.36186612440196,16.6464275938578,-26.3111801406621)) ;
#8925 = CARTESIAN_POINT('Ctrl Pts',(6.35597562166154,16.6474585886992,-26.3079691091064)) ;
#8926 = CARTESIAN_POINT('Ctrl Pts',(6.34245949856352,16.6492439669154,-26.3023795561698)) ;
#8927 = CARTESIAN_POINT('Ctrl Pts',(6.33483452413194,16.65,-26.2999999999999)) ;
#8928 = CARTESIAN_POINT('Ctrl Pts',(6.325,16.65,-26.2999999999999)) ;
#8929 = CARTESIAN_POINT('',(6.325,20.6397935779816,-13.0006880733945)) ;
#8930 = CARTESIAN_POINT('Origin',(-9.5,28.6,33.4)) ;
#8931 = CARTESIAN_POINT('',(-9.5,27.9,33.5)) ;
#8932 = CARTESIAN_POINT('Origin',(-9.5,31.75,25.85)) ;
#8933 = CARTESIAN_POINT('',(-6.325,31.75,25.85)) ;
#8934 = CARTESIAN_POINT('',(-9.5,31.75,25.85)) ;
#8935 = CARTESIAN_POINT('',(-6.325,31.75,14.1625)) ;
#8936 = CARTESIAN_POINT('Origin',(-9.5,18.3909804312853,25.996564592546)) ;
#8937 = CARTESIAN_POINT('',(-6.325,31.2,22.2)) ;
#8938 = CARTESIAN_POINT('',(-9.5,31.2,22.2)) ;
#8939 = CARTESIAN_POINT('Origin',(-6.325,18.3909804312853,25.996564592546)) ;
#8940 = CARTESIAN_POINT('Origin',(-9.5,16.65,-26.3)) ;
#8941 = CARTESIAN_POINT('',(-6.325,16.65,-26.3)) ;
#8942 = CARTESIAN_POINT('',(-9.5,16.65,-26.3)) ;
#8943 = CARTESIAN_POINT('',(-6.325,20.6397935779816,-13.0006880733945)) ;
#8944 = CARTESIAN_POINT('Origin',(-9.5,13.5741698750304,-25.3227636083745)) ;
#8945 = CARTESIAN_POINT('',(-9.36972204690191,13.6,-28.55)) ;
#8946 = CARTESIAN_POINT('',(-9.5,13.6,-28.55)) ;
#8947 = CARTESIAN_POINT('Ctrl Pts',(-6.325,16.65,-26.2999999999999)) ;
#8948 = CARTESIAN_POINT('Ctrl Pts',(-6.33483452413193,16.65,-26.2999999999999)) ;
#8949 = CARTESIAN_POINT('Ctrl Pts',(-6.34245949856349,16.6492439669154,-26.3023795561699)) ;
#8950 = CARTESIAN_POINT('Ctrl Pts',(-6.35597562166151,16.6474585886992,-26.3079691091065)) ;
#8951 = CARTESIAN_POINT('Ctrl Pts',(-6.36186612440198,16.6464275938579,-26.311180140662)) ;
#8952 = CARTESIAN_POINT('Ctrl Pts',(-6.37860103000995,16.6431409047044,-26.3213573070102)) ;
#8953 = CARTESIAN_POINT('Ctrl Pts',(-6.38827974448013,16.6407770204755,-26.3285991010219)) ;
#8954 = CARTESIAN_POINT('Ctrl Pts',(-6.41711081442201,16.6333341653242,-26.3511046831614)) ;
#8955 = CARTESIAN_POINT('Ctrl Pts',(-6.43498907397077,16.6280885098712,-26.3665958960957)) ;
#8956 = CARTESIAN_POINT('Ctrl Pts',(-6.4897590083393,16.611175247101,-26.4152486293163)) ;
#8957 = CARTESIAN_POINT('Ctrl Pts',(-6.52704506600962,16.5986811618034,-26.4494819237855)) ;
#8958 = CARTESIAN_POINT('Ctrl Pts',(-6.64224012239148,16.5576770884375,-26.5557152165318)) ;
#8959 = CARTESIAN_POINT('Ctrl Pts',(-6.72629598955389,16.524579645383,-26.6336670195021)) ;
#8960 = CARTESIAN_POINT('Ctrl Pts',(-6.98513622894906,16.4114752355335,-26.8706894533264)) ;
#8961 = CARTESIAN_POINT('Ctrl Pts',(-7.18160415304355,16.3103729693986,-27.0469270071979)) ;
#8962 = CARTESIAN_POINT('Ctrl Pts',(-7.770084479292,15.9418765716257,-27.5554690453291)) ;
#8963 = CARTESIAN_POINT('Ctrl Pts',(-8.2020248043842,15.5807535317409,-27.9023312808353)) ;
#8964 = CARTESIAN_POINT('Ctrl Pts',(-8.81830342317925,14.8140076105995,-28.324179740912)) ;
#8965 = CARTESIAN_POINT('Ctrl Pts',(-9.06189751586222,14.4233292907506,-28.4655098589506)) ;
#8966 = CARTESIAN_POINT('Ctrl Pts',(-9.28537554981067,13.8692960232194,-28.5392936237713)) ;
#8967 = CARTESIAN_POINT('Ctrl Pts',(-9.33150428640196,13.7352848730332,-28.5489172081766)) ;
#8968 = CARTESIAN_POINT('Ctrl Pts',(-9.36972204690191,13.6,-28.55)) ;
#8969 = CARTESIAN_POINT('Origin',(-6.325,17.5986951224045,-12.0883585367213)) ;
#8970 = CARTESIAN_POINT('Origin',(-6.325,12.6602026834209,-28.55)) ;
#8971 = CARTESIAN_POINT('Ctrl Pts',(-9.5,28.1572902981989,23.1069587159267)) ;
#8972 = CARTESIAN_POINT('Ctrl Pts',(-9.5,28.1804450776062,23.100060067043)) ;
#8973 = CARTESIAN_POINT('Ctrl Pts',(-9.49972422059572,28.203599079597,23.0931615647918)) ;
#8974 = CARTESIAN_POINT('Ctrl Pts',(-9.49851304725432,28.2544365009326,23.0780148814129)) ;
#8975 = CARTESIAN_POINT('Ctrl Pts',(-9.49745895112744,28.282115267648,23.0697680502973)) ;
#8976 = CARTESIAN_POINT('Ctrl Pts',(-9.49333672763735,28.3608494434262,23.0463090289002)) ;
#8977 = CARTESIAN_POINT('Ctrl Pts',(-9.48931972873404,28.4118497186098,23.0311129802741)) ;
#8978 = CARTESIAN_POINT('Ctrl Pts',(-9.47326463912794,28.5643586303556,22.9856702330659)) ;
#8979 = CARTESIAN_POINT('Ctrl Pts',(-9.45723262679847,28.6654075247156,22.9555593489356)) ;
#8980 = CARTESIAN_POINT('Ctrl Pts',(-9.39330812723007,28.9657149615822,22.8660684272212)) ;
#8981 = CARTESIAN_POINT('Ctrl Pts',(-9.32974954840784,29.1613140148454,22.8077745275693)) ;
#8982 = CARTESIAN_POINT('Ctrl Pts',(-9.08425034833606,29.7138633169093,22.6430862375867)) ;
#8983 = CARTESIAN_POINT('Ctrl Pts',(-8.84953554453545,30.0445944579962,22.544493476295)) ;
#8984 = CARTESIAN_POINT('Ctrl Pts',(-8.26103034809262,30.6012160784109,22.378546241529)) ;
#8985 = CARTESIAN_POINT('Ctrl Pts',(-7.91286656008235,30.8217851943076,22.3127786094003)) ;
#8986 = CARTESIAN_POINT('Ctrl Pts',(-7.14791041242474,31.1226151396559,22.2230766109175)) ;
#8987 = CARTESIAN_POINT('Ctrl Pts',(-6.73843153640695,31.2000000000001,22.2000000000002)) ;
#8988 = CARTESIAN_POINT('Ctrl Pts',(-6.325,31.2000000000001,22.2000000000002)) ;
#8989 = CARTESIAN_POINT('Origin',(-6.325,28.575,14.1625)) ;
#8990 = CARTESIAN_POINT('Ctrl Pts',(-6.325,31.75,25.85)) ;
#8991 = CARTESIAN_POINT('Ctrl Pts',(-6.43046239133936,31.75,25.8503682782621)) ;
#8992 = CARTESIAN_POINT('Ctrl Pts',(-6.53592460944136,31.7447410186195,25.8507365565242)) ;
#8993 = CARTESIAN_POINT('Ctrl Pts',(-6.64086381191953,31.7342491279289,25.8511048347863)) ;
#8994 = CARTESIAN_POINT('Ctrl Pts',(-6.74579990719284,31.7237575478987,25.8514731021438)) ;
#8995 = CARTESIAN_POINT('Ctrl Pts',(-6.8502126731198,31.7080334031633,25.8518413695013)) ;
#8996 = CARTESIAN_POINT('Ctrl Pts',(-6.95358450071494,31.6871546435646,25.8522096368589)) ;
#8997 = CARTESIAN_POINT('Ctrl Pts',(-7.05695346822128,31.6662764616389,25.8525778940272)) ;
#8998 = CARTESIAN_POINT('Ctrl Pts',(-7.15928121551033,31.6402440188948,25.8529461511955)) ;
#8999 = CARTESIAN_POINT('Ctrl Pts',(-7.26006049775935,31.6091863597232,25.8533144083638)) ;
#9000 = CARTESIAN_POINT('Ctrl Pts',(-7.3608371872827,31.5781294995648,25.8536826560581)) ;
#9001 = CARTESIAN_POINT('Ctrl Pts',(-7.46006516052103,31.542047783755,25.8540509037523)) ;
#9002 = CARTESIAN_POINT('Ctrl Pts',(-7.55725256368973,31.5011200623488,25.8544191514466)) ;
#9003 = CARTESIAN_POINT('Ctrl Pts',(-7.6544376551641,31.4601933144471,25.8547873903817)) ;
#9004 = CARTESIAN_POINT('Ctrl Pts',(-7.74958195456512,31.4144209260739,25.8551556293169)) ;
#9005 = CARTESIAN_POINT('Ctrl Pts',(-7.84221387248779,31.364029771288,25.855523868252)) ;
#9006 = CARTESIAN_POINT('Ctrl Pts',(-7.93484376682315,31.3136397173203,25.8558920991428)) ;
#9007 = CARTESIAN_POINT('Ctrl Pts',(-8.02496108536813,31.2586312643688,25.8562603300335)) ;
#9008 = CARTESIAN_POINT('Ctrl Pts',(-8.11211917478788,31.1992770538008,25.8566285609243)) ;
#9009 = CARTESIAN_POINT('Ctrl Pts',(-8.19927552929977,31.1399240246962,25.8569967844854)) ;
#9010 = CARTESIAN_POINT('Ctrl Pts',(-8.28347248641858,31.0762256060054,25.8573650080464)) ;
#9011 = CARTESIAN_POINT('Ctrl Pts',(-8.36429275280517,31.0084974970927,25.8577332316074)) ;
#9012 = CARTESIAN_POINT('Ctrl Pts',(-8.44511156722147,30.9407706049441,25.8581014485532)) ;
#9013 = CARTESIAN_POINT('Ctrl Pts',(-8.52255354698811,30.8690143898423,25.8584696654989)) ;
#9014 = CARTESIAN_POINT('Ctrl Pts',(-8.59623489126445,30.7935844740967,25.8588378824447)) ;
#9015 = CARTESIAN_POINT('Ctrl Pts',(-8.66992797872015,30.718142536488,25.8592061580761)) ;
#9016 = CARTESIAN_POINT('Ctrl Pts',(-8.73985898883772,30.6390259739448,25.8595744337075)) ;
#9017 = CARTESIAN_POINT('Ctrl Pts',(-8.80568123466801,30.5566270113132,25.8599427093388)) ;
#9018 = CARTESIAN_POINT('Ctrl Pts',(-8.87149977051629,30.4742326929879,25.8603109642129)) ;
#9019 = CARTESIAN_POINT('Ctrl Pts',(-8.93320978941985,30.3885566155287,25.8606792190869)) ;
#9020 = CARTESIAN_POINT('Ctrl Pts',(-8.9905053948943,30.3000234751415,25.861047473961)) ;
#9021 = CARTESIAN_POINT('Ctrl Pts',(-9.04779821585521,30.2114946373833,25.8614157109381)) ;
#9022 = CARTESIAN_POINT('Ctrl Pts',(-9.10067686465044,30.1201093053544,25.8617839479153)) ;
#9023 = CARTESIAN_POINT('Ctrl Pts',(-9.14887924732489,30.0263204320645,25.8621521848925)) ;
#9024 = CARTESIAN_POINT('Ctrl Pts',(-9.19707966154245,29.9325353888623,25.8625204068319)) ;
#9025 = CARTESIAN_POINT('Ctrl Pts',(-9.24060403361372,29.836347308807,25.8628886287713)) ;
#9026 = CARTESIAN_POINT('Ctrl Pts',(-9.27923665181417,29.7382329109331,25.8632568507106)) ;
#9027 = CARTESIAN_POINT('Ctrl Pts',(-9.31787436355134,29.6401055771177,25.8636251211984)) ;
#9028 = CARTESIAN_POINT('Ctrl Pts',(-9.35161890345644,29.5400517393644,25.8639933916862)) ;
#9029 = CARTESIAN_POINT('Ctrl Pts',(-9.38030298572493,29.4385674064138,25.864361662174)) ;
#9030 = CARTESIAN_POINT('Ctrl Pts',(-9.40898416208845,29.3370933545602,25.8647298953533)) ;
#9031 = CARTESIAN_POINT('Ctrl Pts',(-9.43260581273696,29.234189430832,25.8650981285326)) ;
#9032 = CARTESIAN_POINT('Ctrl Pts',(-9.45105085895399,29.1303656698366,25.8654663617119)) ;
#9033 = CARTESIAN_POINT('Ctrl Pts',(-9.46949728240109,29.0265341566673,25.865834622386)) ;
#9034 = CARTESIAN_POINT('Ctrl Pts',(-9.4827662671269,28.9217830097633,25.86620288306)) ;
#9035 = CARTESIAN_POINT('Ctrl Pts',(-9.49079203672237,28.8166314967574,25.8665711437341)) ;
#9036 = CARTESIAN_POINT('Ctrl Pts',(-9.49692771002532,28.7362435260538,25.8668526777551)) ;
#9037 = CARTESIAN_POINT('Ctrl Pts',(-9.5,28.6556217856458,25.8671342117762)) ;
#9038 = CARTESIAN_POINT('Ctrl Pts',(-9.5,28.575,25.8674157457972)) ;
#9039 = CARTESIAN_POINT('Origin',(-6.325,18.3909804312853,25.996564592546)) ;
#9040 = CARTESIAN_POINT('Origin',(-9.5,3.,-28.55)) ;
#9041 = CARTESIAN_POINT('Origin',(-16.75,0.,12.99)) ;
#9042 = CARTESIAN_POINT('',(-16.75,0.,12.99)) ;
#9043 = CARTESIAN_POINT('',(-16.75,0.,12.99)) ;
#9044 = CARTESIAN_POINT('',(-18.25,0.,12.99)) ;
#9045 = CARTESIAN_POINT('Origin',(-16.75,0.,10.325)) ;
#9046 = CARTESIAN_POINT('Origin',(-16.75,0.,10.325)) ;
#9047 = CARTESIAN_POINT('Origin',(18.25,0.,12.99)) ;
#9048 = CARTESIAN_POINT('',(18.25,0.,12.99)) ;
#9049 = CARTESIAN_POINT('',(18.25,0.,12.99)) ;
#9050 = CARTESIAN_POINT('',(16.75,0.,12.99)) ;
#9051 = CARTESIAN_POINT('Origin',(18.25,0.,10.325)) ;
#9052 = CARTESIAN_POINT('Origin',(18.25,0.,10.325)) ;
#9053 = CARTESIAN_POINT('Origin',(-24.75,0.,-14.3)) ;
#9054 = CARTESIAN_POINT('',(-24.75,0.,-14.3)) ;
#9055 = CARTESIAN_POINT('',(-24.75,0.,-14.3)) ;
#9056 = CARTESIAN_POINT('',(-24.75,0.,33.25)) ;
#9057 = CARTESIAN_POINT('',(-24.75,0.,33.25)) ;
#9058 = CARTESIAN_POINT('',(-24.75,0.,33.25)) ;
#9059 = CARTESIAN_POINT('Origin',(-21.664129241231,0.,-14.3226323462975)) ;
#9060 = CARTESIAN_POINT('',(-23.8,0.,-16.55)) ;
#9061 = CARTESIAN_POINT('',(-23.8,0.,-16.55)) ;
#9062 = CARTESIAN_POINT('Origin',(-21.664129241231,0.,-14.3226323462975)) ;
#9063 = CARTESIAN_POINT('Origin',(-11.7,0.,-28.65)) ;
#9064 = CARTESIAN_POINT('',(-11.7,0.,-28.65)) ;
#9065 = CARTESIAN_POINT('',(-11.7,0.,-28.65)) ;
#9066 = CARTESIAN_POINT('',(-23.8,0.,-16.55)) ;
#9067 = CARTESIAN_POINT('Origin',(1.11022302462516E-15,0.,-16.8941925465839)) ;
#9068 = CARTESIAN_POINT('',(11.7,0.,-28.65)) ;
#9069 = CARTESIAN_POINT('',(11.7,0.,-28.65)) ;
#9070 = CARTESIAN_POINT('Origin',(1.11022302462516E-15,0.,-16.8941925465839)) ;
#9071 = CARTESIAN_POINT('Origin',(23.8,0.,-16.55)) ;
#9072 = CARTESIAN_POINT('',(23.8,0.,-16.55)) ;
#9073 = CARTESIAN_POINT('',(23.8,0.,-16.55)) ;
#9074 = CARTESIAN_POINT('',(11.7,0.,-28.65)) ;
#9075 = CARTESIAN_POINT('Origin',(21.4457388066382,0.,-14.2304230516917)) ;
#9076 = CARTESIAN_POINT('',(24.75,0.,-14.3)) ;
#9077 = CARTESIAN_POINT('',(24.75,0.,-14.3)) ;
#9078 = CARTESIAN_POINT('Origin',(21.4457388066382,0.,-14.2304230516917)) ;
#9079 = CARTESIAN_POINT('Origin',(24.75,0.,33.25)) ;
#9080 = CARTESIAN_POINT('',(24.75,0.,33.25)) ;
#9081 = CARTESIAN_POINT('',(24.75,0.,33.25)) ;
#9082 = CARTESIAN_POINT('',(24.75,0.,-14.3)) ;
#9083 = CARTESIAN_POINT('Origin',(24.5,0.,33.25)) ;
#9084 = CARTESIAN_POINT('',(24.5,0.,33.5)) ;
#9085 = CARTESIAN_POINT('',(24.5,0.,33.5)) ;
#9086 = CARTESIAN_POINT('Origin',(24.5,0.,33.25)) ;
#9087 = CARTESIAN_POINT('Origin',(-24.5,0.,33.5)) ;
#9088 = CARTESIAN_POINT('',(-24.5,0.,33.5)) ;
#9089 = CARTESIAN_POINT('',(-24.5,0.,33.5)) ;
#9090 = CARTESIAN_POINT('',(24.5,0.,33.5)) ;
#9091 = CARTESIAN_POINT('Origin',(-24.5,0.,33.25)) ;
#9092 = CARTESIAN_POINT('Origin',(-24.5,0.,33.25)) ;
#9093 = CARTESIAN_POINT('Origin',(-4.14968943118765E-5,0.,0.0099999999999989)) ;
#9094 = CARTESIAN_POINT('',(0.,0.,0.)) ;
#9095 = CARTESIAN_POINT('Origin',(-9.75,3.55,44.8475)) ;
#9096 = CARTESIAN_POINT('',(-9.73166789581674,3.300673038048,52.4412514394322)) ;
#9097 = CARTESIAN_POINT('',(-9.5,3.55,51.7196985577435)) ;
#9098 = CARTESIAN_POINT('Ctrl Pts',(-9.73166789581674,3.300673038048,52.4412514394322)) ;
#9099 = CARTESIAN_POINT('Ctrl Pts',(-9.72011624748849,3.30152238871182,52.4296997911002)) ;
#9100 = CARTESIAN_POINT('Ctrl Pts',(-9.71077453059008,3.30297344738984,52.4127655658232)) ;
#9101 = CARTESIAN_POINT('Ctrl Pts',(-9.66740696188674,3.31125291954623,52.3320464604663)) ;
#9102 = CARTESIAN_POINT('Ctrl Pts',(-9.63485752215083,3.32587980802581,52.2484283731037)) ;
#9103 = CARTESIAN_POINT('Ctrl Pts',(-9.58078548283598,3.3628440108946,52.104753223308)) ;
#9104 = CARTESIAN_POINT('Ctrl Pts',(-9.55334337963797,3.39036468556239,52.0234232206868)) ;
#9105 = CARTESIAN_POINT('Ctrl Pts',(-9.51285745751298,3.4610024800945,51.8649901763511)) ;
#9106 = CARTESIAN_POINT('Ctrl Pts',(-9.5,3.50416452181587,51.7878595996225)) ;
#9107 = CARTESIAN_POINT('Ctrl Pts',(-9.5,3.55,51.7196985577435)) ;
#9108 = CARTESIAN_POINT('',(-9.5,3.55,35.75)) ;
#9109 = CARTESIAN_POINT('',(-9.5,3.55,44.8475)) ;
#9110 = CARTESIAN_POINT('',(-9.75,3.3,35.75)) ;
#9111 = CARTESIAN_POINT('Origin',(-9.75,3.55,35.75)) ;
#9112 = CARTESIAN_POINT('',(-9.75,3.3,52.4595835436154)) ;
#9113 = CARTESIAN_POINT('',(-9.75,3.3,44.8475)) ;
#9114 = CARTESIAN_POINT('Origin',(-9.75,3.55,52.4595835436154)) ;
#9115 = CARTESIAN_POINT('Origin',(-9.75,3.05,35.75)) ;
#9116 = CARTESIAN_POINT('',(-9.5,3.48301270189222,35.5)) ;
#9117 = CARTESIAN_POINT('',(-9.75,3.05,35.5)) ;
#9118 = CARTESIAN_POINT('Ctrl Pts',(-9.5,3.48301270189222,35.5)) ;
#9119 = CARTESIAN_POINT('Ctrl Pts',(-9.5,3.41929334642333,35.5)) ;
#9120 = CARTESIAN_POINT('Ctrl Pts',(-9.52239299997444,3.34618261828772,35.5)) ;
#9121 = CARTESIAN_POINT('Ctrl Pts',(-9.59902182095282,3.203805818051,35.5)) ;
#9122 = CARTESIAN_POINT('Ctrl Pts',(-9.68072544447976,3.11927455552024,35.5)) ;
#9123 = CARTESIAN_POINT('Ctrl Pts',(-9.75,3.05,35.5)) ;
#9124 = CARTESIAN_POINT('Origin',(-9.75,3.05,35.75)) ;
#9125 = CARTESIAN_POINT('Origin',(-9.5,3.05,35.75)) ;
#9126 = CARTESIAN_POINT('Origin',(-9.5,14.6475105520359,44.075)) ;
#9127 = CARTESIAN_POINT('',(-9.5,4.45,51.1)) ;
#9128 = CARTESIAN_POINT('Origin',(-9.5,4.78534007458122,52.5504136037216)) ;
#9129 = CARTESIAN_POINT('',(-9.5,22.05,46.65)) ;
#9130 = CARTESIAN_POINT('',(-9.5,22.05,46.65)) ;
#9131 = CARTESIAN_POINT('',(-9.5,20.65,35.5)) ;
#9132 = CARTESIAN_POINT('Origin',(-9.5,20.629520265574,41.1654638231566)) ;
#9133 = CARTESIAN_POINT('',(-9.5,3.,35.5)) ;
#9134 = CARTESIAN_POINT('',(-9.5,19.79,40.28)) ;
#9135 = CARTESIAN_POINT('Origin',(-9.5,19.79,38.695)) ;
#9136 = CARTESIAN_POINT('Origin',(9.75,3.05,35.75)) ;
#9137 = CARTESIAN_POINT('',(9.5,3.55,35.75)) ;
#9138 = CARTESIAN_POINT('',(9.75,3.3,35.75)) ;
#9139 = CARTESIAN_POINT('Origin',(9.75,3.55,35.75)) ;
#9140 = CARTESIAN_POINT('',(9.75,3.05,35.5)) ;
#9141 = CARTESIAN_POINT('Origin',(9.75,3.05,35.75)) ;
#9142 = CARTESIAN_POINT('',(9.5,3.48301270189222,35.5)) ;
#9143 = CARTESIAN_POINT('Ctrl Pts',(9.75,3.05,35.5)) ;
#9144 = CARTESIAN_POINT('Ctrl Pts',(9.68072544447976,3.11927455552024,35.5)) ;
#9145 = CARTESIAN_POINT('Ctrl Pts',(9.59902182095282,3.203805818051,35.5)) ;
#9146 = CARTESIAN_POINT('Ctrl Pts',(9.52239299997444,3.34618261828772,35.5)) ;
#9147 = CARTESIAN_POINT('Ctrl Pts',(9.5,3.41929334642333,35.5)) ;
#9148 = CARTESIAN_POINT('Ctrl Pts',(9.5,3.48301270189222,35.5)) ;
#9149 = CARTESIAN_POINT('Origin',(9.5,3.05,35.75)) ;
#9150 = CARTESIAN_POINT('Origin',(9.75,3.55,44.8475)) ;
#9151 = CARTESIAN_POINT('',(9.75,3.3,52.4595835436154)) ;
#9152 = CARTESIAN_POINT('',(9.73166789577781,3.30067303805086,52.4412514393933)) ;
#9153 = CARTESIAN_POINT('Origin',(9.75,3.55,52.4595835436154)) ;
#9154 = CARTESIAN_POINT('',(9.75,3.3,44.8475)) ;
#9155 = CARTESIAN_POINT('',(9.5,3.55,51.7196985577435)) ;
#9156 = CARTESIAN_POINT('',(9.5,3.55,44.8475)) ;
#9157 = CARTESIAN_POINT('Ctrl Pts',(9.5,3.55,51.7196985577435)) ;
#9158 = CARTESIAN_POINT('Ctrl Pts',(9.5,3.50416452181587,51.7878595996225)) ;
#9159 = CARTESIAN_POINT('Ctrl Pts',(9.51285745751298,3.4610024800945,51.8649901763511)) ;
#9160 = CARTESIAN_POINT('Ctrl Pts',(9.55334337963797,3.39036468556239,52.0234232206868)) ;
#9161 = CARTESIAN_POINT('Ctrl Pts',(9.58078548283598,3.3628440108946,52.104753223308)) ;
#9162 = CARTESIAN_POINT('Ctrl Pts',(9.63485752215083,3.32587980802581,52.2484283731037)) ;
#9163 = CARTESIAN_POINT('Ctrl Pts',(9.66740696188674,3.31125291954623,52.3320464604663)) ;
#9164 = CARTESIAN_POINT('Ctrl Pts',(9.71077453058148,3.30297344739148,52.4127655658072)) ;
#9165 = CARTESIAN_POINT('Ctrl Pts',(9.72011624746926,3.30152238871505,52.4296997910605)) ;
#9166 = CARTESIAN_POINT('Ctrl Pts',(9.7316678957778,3.30067303805086,52.4412514393933)) ;
#9167 = CARTESIAN_POINT('Origin',(9.5,14.6475105520359,44.075)) ;
#9168 = CARTESIAN_POINT('',(9.5,20.65,35.5)) ;
#9169 = CARTESIAN_POINT('',(9.5,3.,35.5)) ;
#9170 = CARTESIAN_POINT('',(9.5,22.05,46.65)) ;
#9171 = CARTESIAN_POINT('Origin',(9.5,20.629520265574,41.1654638231566)) ;
#9172 = CARTESIAN_POINT('',(9.5,4.45,51.1)) ;
#9173 = CARTESIAN_POINT('',(9.5,22.05,46.65)) ;
#9174 = CARTESIAN_POINT('Origin',(9.5,4.78534007458122,52.5504136037216)) ;
#9175 = CARTESIAN_POINT('',(9.5,19.79,40.28)) ;
#9176 = CARTESIAN_POINT('Origin',(9.5,19.79,38.695)) ;
#9177 = CARTESIAN_POINT('Origin',(-19.8,3.05,45.625)) ;
#9178 = CARTESIAN_POINT('',(-19.8,3.3,48.54)) ;
#9179 = CARTESIAN_POINT('',(-19.8,3.05,48.29)) ;
#9180 = CARTESIAN_POINT('Origin',(-19.8,3.05,48.54)) ;
#9181 = CARTESIAN_POINT('',(-19.8,3.05,42.96)) ;
#9182 = CARTESIAN_POINT('Origin',(-19.8,3.05,45.625)) ;
#9183 = CARTESIAN_POINT('',(-19.8,3.3,42.71)) ;
#9184 = CARTESIAN_POINT('Origin',(-19.8,3.05,42.71)) ;
#9185 = CARTESIAN_POINT('Origin',(-19.8,3.3,45.625)) ;
#9186 = CARTESIAN_POINT('Origin',(-9.89996640571749,3.05,42.71)) ;
#9187 = CARTESIAN_POINT('',(-16.75,3.05,42.96)) ;
#9188 = CARTESIAN_POINT('',(-16.75,3.3,42.71)) ;
#9189 = CARTESIAN_POINT('Origin',(-16.75,3.05,42.71)) ;
#9190 = CARTESIAN_POINT('',(-9.89996640571749,3.3,42.71)) ;
#9191 = CARTESIAN_POINT('',(-9.89996640571749,3.05,42.96)) ;
#9192 = CARTESIAN_POINT('Origin',(-16.75,3.05,45.625)) ;
#9193 = CARTESIAN_POINT('',(-16.75,3.05,48.29)) ;
#9194 = CARTESIAN_POINT('',(-16.75,3.3,48.54)) ;
#9195 = CARTESIAN_POINT('Origin',(-16.75,3.05,48.54)) ;
#9196 = CARTESIAN_POINT('Origin',(-16.75,3.3,45.625)) ;
#9197 = CARTESIAN_POINT('Origin',(-16.75,3.05,45.625)) ;
#9198 = CARTESIAN_POINT('Origin',(-8.3749664057175,3.05,48.54)) ;
#9199 = CARTESIAN_POINT('',(-8.3749664057175,3.3,48.54)) ;
#9200 = CARTESIAN_POINT('',(-8.3749664057175,3.05,48.29)) ;
#9201 = CARTESIAN_POINT('Origin',(-19.8,0.,42.96)) ;
#9202 = CARTESIAN_POINT('',(-19.8,0.,42.96)) ;
#9203 = CARTESIAN_POINT('',(-19.8,0.,42.96)) ;
#9204 = CARTESIAN_POINT('',(-16.75,0.,42.96)) ;
#9205 = CARTESIAN_POINT('',(-16.75,0.,42.96)) ;
#9206 = CARTESIAN_POINT('',(-16.75,0.,42.96)) ;
#9207 = CARTESIAN_POINT('Origin',(-19.8,0.,45.625)) ;
#9208 = CARTESIAN_POINT('',(-19.8,0.,48.29)) ;
#9209 = CARTESIAN_POINT('',(-19.8,0.,48.29)) ;
#9210 = CARTESIAN_POINT('Origin',(-19.8,0.,45.625)) ;
#9211 = CARTESIAN_POINT('Origin',(6.71885650094239E-5,3.3,45.62)) ;
#9212 = CARTESIAN_POINT('',(-24.1,3.3,35.75)) ;
#9213 = CARTESIAN_POINT('',(12.0500335942825,3.3,35.75)) ;
#9214 = CARTESIAN_POINT('',(-24.5,3.3,36.15)) ;
#9215 = CARTESIAN_POINT('Origin',(-24.1,3.3,36.15)) ;
#9216 = CARTESIAN_POINT('',(-24.5,3.3,45.0477339100826)) ;
#9217 = CARTESIAN_POINT('',(-24.5,3.3,40.885)) ;
#9218 = CARTESIAN_POINT('',(-21.0874960519899,3.3,50.4767448507153)) ;
#9219 = CARTESIAN_POINT('Origin',(-18.2944180372184,3.3,44.9341033685178)) ;
#9220 = CARTESIAN_POINT('',(21.0902564701365,3.3,50.4753536112778)) ;
#9221 = CARTESIAN_POINT('Origin',(0.,3.3,8.63269841269837)) ;
#9222 = CARTESIAN_POINT('',(24.4999999432639,3.3,45.0508225837103)) ;
#9223 = CARTESIAN_POINT('Origin',(18.5438728059353,3.3,45.0908404355877)) ;
#9224 = CARTESIAN_POINT('',(24.5,3.3,36.15)) ;
#9225 = CARTESIAN_POINT('',(24.5,3.3,45.335)) ;
#9226 = CARTESIAN_POINT('',(24.1,3.3,35.75)) ;
#9227 = CARTESIAN_POINT('Origin',(24.1,3.3,36.15)) ;
#9228 = CARTESIAN_POINT('',(12.0500335942825,3.3,35.75)) ;
#9229 = CARTESIAN_POINT('',(-9.5,3.3,52.4595835436154)) ;
#9230 = CARTESIAN_POINT('',(16.75,3.3,42.71)) ;
#9231 = CARTESIAN_POINT('',(16.75,3.3,48.54)) ;
#9232 = CARTESIAN_POINT('Origin',(16.75,3.3,45.625)) ;
#9233 = CARTESIAN_POINT('',(19.8,3.3,42.71)) ;
#9234 = CARTESIAN_POINT('',(8.3750335942825,3.3,42.71)) ;
#9235 = CARTESIAN_POINT('',(19.8,3.3,48.54)) ;
#9236 = CARTESIAN_POINT('Origin',(19.8,3.3,45.625)) ;
#9237 = CARTESIAN_POINT('',(9.9000335942825,3.3,48.54)) ;
#9238 = CARTESIAN_POINT('Origin',(16.75,3.05,45.625)) ;
#9239 = CARTESIAN_POINT('',(16.75,3.05,48.29)) ;
#9240 = CARTESIAN_POINT('Origin',(16.75,3.05,48.54)) ;
#9241 = CARTESIAN_POINT('',(16.75,3.05,42.96)) ;
#9242 = CARTESIAN_POINT('Origin',(16.75,3.05,45.625)) ;
#9243 = CARTESIAN_POINT('Origin',(16.75,3.05,42.71)) ;
#9244 = CARTESIAN_POINT('Origin',(8.3750335942825,3.05,42.71)) ;
#9245 = CARTESIAN_POINT('',(19.8,3.05,42.96)) ;
#9246 = CARTESIAN_POINT('Origin',(19.8,3.05,42.71)) ;
#9247 = CARTESIAN_POINT('',(8.3750335942825,3.05,42.96)) ;
#9248 = CARTESIAN_POINT('Origin',(19.8,3.05,45.625)) ;
#9249 = CARTESIAN_POINT('',(19.8,3.05,48.29)) ;
#9250 = CARTESIAN_POINT('Origin',(19.8,3.05,48.54)) ;
#9251 = CARTESIAN_POINT('Origin',(19.8,3.05,45.625)) ;
#9252 = CARTESIAN_POINT('Origin',(9.9000335942825,3.05,48.54)) ;
#9253 = CARTESIAN_POINT('',(9.9000335942825,3.05,48.29)) ;
#9254 = CARTESIAN_POINT('Origin',(16.75,0.,42.96)) ;
#9255 = CARTESIAN_POINT('',(16.75,0.,42.96)) ;
#9256 = CARTESIAN_POINT('',(16.75,0.,42.96)) ;
#9257 = CARTESIAN_POINT('',(19.8,0.,42.96)) ;
#9258 = CARTESIAN_POINT('',(19.8,0.,42.96)) ;
#9259 = CARTESIAN_POINT('',(19.8,0.,42.96)) ;
#9260 = CARTESIAN_POINT('Origin',(16.75,0.,45.625)) ;
#9261 = CARTESIAN_POINT('',(16.75,0.,48.29)) ;
#9262 = CARTESIAN_POINT('',(16.75,0.,48.29)) ;
#9263 = CARTESIAN_POINT('Origin',(16.75,0.,45.625)) ;
#9264 = CARTESIAN_POINT('Origin',(-9.5,3.55,52.4595835436154)) ;
#9265 = CARTESIAN_POINT('',(-9.5,3.30067303804748,52.4412514394393)) ;
#9266 = CARTESIAN_POINT('Origin',(-9.5,4.78534007458122,52.5504136037216)) ;
#9267 = CARTESIAN_POINT('',(-9.5,4.45,51.1)) ;
#9268 = CARTESIAN_POINT('Origin',(18.5438728059353,3.05,45.0908404355877)) ;
#9269 = CARTESIAN_POINT('',(21.2,3.05,50.7)) ;
#9270 = CARTESIAN_POINT('',(24.75,3.05,45.05)) ;
#9271 = CARTESIAN_POINT('Origin',(18.5438728059353,3.05,45.0908404355877)) ;
#9272 = CARTESIAN_POINT('Ctrl Pts',(24.75,3.05,45.05)) ;
#9273 = CARTESIAN_POINT('Ctrl Pts',(24.7499997649959,3.06636246173745,45.0499642886908)) ;
#9274 = CARTESIAN_POINT('Ctrl Pts',(24.7483880426071,3.08272451888078,45.0499391822158)) ;
#9275 = CARTESIAN_POINT('Ctrl Pts',(24.7451957187188,3.09877258050403,45.049924559718)) ;
#9276 = CARTESIAN_POINT('Ctrl Pts',(24.742135735277,3.11415535636217,45.0499105434081)) ;
#9277 = CARTESIAN_POINT('Ctrl Pts',(24.7376239954586,3.12924901976136,45.049906156751)) ;
#9278 = CARTESIAN_POINT('Ctrl Pts',(24.7317399828519,3.14378765298013,45.0499109447592)) ;
#9279 = CARTESIAN_POINT('Ctrl Pts',(24.7258570786838,3.15832354739046,45.0499157318653)) ;
#9280 = CARTESIAN_POINT('Ctrl Pts',(24.7186026657308,3.17230401465796,45.0499296888126)) ;
#9281 = CARTESIAN_POINT('Ctrl Pts',(24.7101044996307,3.18548284147049,45.0499520344104)) ;
#9282 = CARTESIAN_POINT('Ctrl Pts',(24.7016076986088,3.19865955134022,45.0499743764187)) ;
#9283 = CARTESIAN_POINT('Ctrl Pts',(24.6918678995193,3.211034329459,45.0500051022664)) ;
#9284 = CARTESIAN_POINT('Ctrl Pts',(24.6810565738722,3.22238931032504,45.0500431309344)) ;
#9285 = CARTESIAN_POINT('Ctrl Pts',(24.6702466852255,3.23374278193012,45.0500811545477)) ;
#9286 = CARTESIAN_POINT('Ctrl Pts',(24.6583660062662,3.24407625489886,45.0501264762469)) ;
#9287 = CARTESIAN_POINT('Ctrl Pts',(24.6456236446434,3.25320785025283,45.0501777521907)) ;
#9288 = CARTESIAN_POINT('Ctrl Pts',(24.6328768472724,3.26234262440984,45.0502290459843)) ;
#9289 = CARTESIAN_POINT('Ctrl Pts',(24.6192682971389,3.27027430056404,45.0502862948054)) ;
#9290 = CARTESIAN_POINT('Ctrl Pts',(24.6050376799198,3.27686317695211,45.0503479362075)) ;
#9291 = CARTESIAN_POINT('Ctrl Pts',(24.5908114805106,3.28345000786299,45.0504095584734)) ;
#9292 = CARTESIAN_POINT('Ctrl Pts',(24.575964194553,3.28869460036439,45.0504755667426)) ;
#9293 = CARTESIAN_POINT('Ctrl Pts',(24.5607571642129,3.29250463772944,45.050544237254)) ;
#9294 = CARTESIAN_POINT('Ctrl Pts',(24.5455488731175,3.29631499096976,45.0506129134587)) ;
#9295 = CARTESIAN_POINT('Ctrl Pts',(24.5299814118393,3.29869039164851,45.0506842481721)) ;
#9296 = CARTESIAN_POINT('Ctrl Pts',(24.5143288443927,3.29958902042781,45.0507564146933)) ;
#9297 = CARTESIAN_POINT('Ctrl Pts',(24.5095577809545,3.29986293171604,45.0507784117907)) ;
#9298 = CARTESIAN_POINT('Ctrl Pts',(24.5047788624715,3.3,45.0508004856938)) ;
#9299 = CARTESIAN_POINT('Ctrl Pts',(24.4999999432639,3.3,45.0508225837103)) ;
#9300 = CARTESIAN_POINT('Ctrl Pts',(21.0902564701365,3.3,50.4753536112778)) ;
#9301 = CARTESIAN_POINT('Ctrl Pts',(21.0907463180989,3.3,50.4763566221903)) ;
#9302 = CARTESIAN_POINT('Ctrl Pts',(21.09123616212,3.29999252528887,50.4773596211075)) ;
#9303 = CARTESIAN_POINT('Ctrl Pts',(21.1060035602585,3.29954182407199,50.5075970557322)) ;
#9304 = CARTESIAN_POINT('Ctrl Pts',(21.1201089113617,3.29275962387286,50.5364754558814)) ;
#9305 = CARTESIAN_POINT('Ctrl Pts',(21.1463954963948,3.26725755617282,50.5902876319832)) ;
#9306 = CARTESIAN_POINT('Ctrl Pts',(21.1583244312364,3.24877490065223,50.6147049771605)) ;
#9307 = CARTESIAN_POINT('Ctrl Pts',(21.1784011784248,3.20243491264089,50.6557973965193)) ;
#9308 = CARTESIAN_POINT('Ctrl Pts',(21.1863573189541,3.17502132423592,50.6720802410836)) ;
#9309 = CARTESIAN_POINT('Ctrl Pts',(21.1972085288292,3.11479146985681,50.6942875251967)) ;
#9310 = CARTESIAN_POINT('Ctrl Pts',(21.1999999999996,3.0825514085482,50.7000000000002)) ;
#9311 = CARTESIAN_POINT('Ctrl Pts',(21.1999999999996,3.05,50.7000000000002)) ;
#9312 = CARTESIAN_POINT('Origin',(24.5,3.05,45.335)) ;
#9313 = CARTESIAN_POINT('',(24.75,3.05,36.15)) ;
#9314 = CARTESIAN_POINT('',(24.75,3.05,45.335)) ;
#9315 = CARTESIAN_POINT('Origin',(24.5,3.05,36.15)) ;
#9316 = CARTESIAN_POINT('Origin',(24.1,3.05,36.15)) ;
#9317 = CARTESIAN_POINT('',(24.1,3.05,35.5)) ;
#9318 = CARTESIAN_POINT('Origin',(24.1,3.05,35.75)) ;
#9319 = CARTESIAN_POINT('Origin',(24.1,3.05,36.15)) ;
#9320 = CARTESIAN_POINT('Origin',(12.0500335942825,3.05,35.75)) ;
#9321 = CARTESIAN_POINT('',(12.0500335942825,3.05,35.5)) ;
#9322 = CARTESIAN_POINT('Origin',(-18.2944180372184,3.05,44.9341033685178)) ;
#9323 = CARTESIAN_POINT('',(-24.75,3.05,45.05)) ;
#9324 = CARTESIAN_POINT('',(-21.2,3.05,50.7)) ;
#9325 = CARTESIAN_POINT('Origin',(-18.2944180372184,3.05,44.9341033685178)) ;
#9326 = CARTESIAN_POINT('Origin',(-21.0874960519899,3.05,50.4767448507153)) ;
#9327 = CARTESIAN_POINT('Ctrl Pts',(-24.5,3.3,45.0477339100826)) ;
#9328 = CARTESIAN_POINT('Ctrl Pts',(-24.5012372116335,3.3,45.0477452364374)) ;
#9329 = CARTESIAN_POINT('Ctrl Pts',(-24.5024744062464,3.29999081584422,45.0477565609417)) ;
#9330 = CARTESIAN_POINT('Ctrl Pts',(-24.5361188401082,3.29949127800647,45.048064475043)) ;
#9331 = CARTESIAN_POINT('Ctrl Pts',(-24.5681256225385,3.29271255013592,45.0483562015273)) ;
#9332 = CARTESIAN_POINT('Ctrl Pts',(-24.6278967898402,3.26726052961233,45.04889912374)) ;
#9333 = CARTESIAN_POINT('Ctrl Pts',(-24.6550706061608,3.24877842887715,45.0491449678964)) ;
#9334 = CARTESIAN_POINT('Ctrl Pts',(-24.7008035019926,3.2024389100284,45.0495577649017)) ;
#9335 = CARTESIAN_POINT('Ctrl Pts',(-24.7189257200146,3.17502490071193,45.0497208021766)) ;
#9336 = CARTESIAN_POINT('Ctrl Pts',(-24.7436420186525,3.11479366304012,45.0499429715952)) ;
#9337 = CARTESIAN_POINT('Ctrl Pts',(-24.75,3.08255247821287,45.05)) ;
#9338 = CARTESIAN_POINT('Ctrl Pts',(-24.75,3.05,45.05)) ;
#9339 = CARTESIAN_POINT('Origin',(0.,3.05,8.63269841269837)) ;
#9340 = CARTESIAN_POINT('Origin',(0.,3.05,8.63269841269837)) ;
#9341 = CARTESIAN_POINT('Origin',(12.0500335942825,3.05,35.75)) ;
#9342 = CARTESIAN_POINT('',(-24.1,3.05,35.5)) ;
#9343 = CARTESIAN_POINT('',(12.0500335942825,3.05,35.5)) ;
#9344 = CARTESIAN_POINT('Origin',(-24.1,3.05,35.75)) ;
#9345 = CARTESIAN_POINT('Origin',(-24.1,3.05,36.15)) ;
#9346 = CARTESIAN_POINT('',(-24.75,3.05,36.15)) ;
#9347 = CARTESIAN_POINT('Origin',(-24.5,3.05,36.15)) ;
#9348 = CARTESIAN_POINT('Origin',(-24.1,3.05,36.15)) ;
#9349 = CARTESIAN_POINT('Origin',(-24.5,3.05,40.885)) ;
#9350 = CARTESIAN_POINT('',(-24.75,3.05,40.885)) ;
#9351 = CARTESIAN_POINT('Origin',(24.1,0.,35.5)) ;
#9352 = CARTESIAN_POINT('',(24.1,0.,35.5)) ;
#9353 = CARTESIAN_POINT('',(24.1,0.,35.5)) ;
#9354 = CARTESIAN_POINT('',(6.95,0.,35.5)) ;
#9355 = CARTESIAN_POINT('',(-24.1,0.,35.5)) ;
#9356 = CARTESIAN_POINT('',(6.95,20.65,35.5)) ;
#9357 = CARTESIAN_POINT('',(6.95,7.5,35.5)) ;
#9358 = CARTESIAN_POINT('',(-9.5,20.65,35.5)) ;
#9359 = CARTESIAN_POINT('Origin',(24.1,0.,36.15)) ;
#9360 = CARTESIAN_POINT('',(24.75,0.,36.15)) ;
#9361 = CARTESIAN_POINT('',(24.75,0.,36.15)) ;
#9362 = CARTESIAN_POINT('Origin',(24.1,0.,36.15)) ;
#9363 = CARTESIAN_POINT('Origin',(24.75,0.,45.05)) ;
#9364 = CARTESIAN_POINT('',(24.75,0.,45.05)) ;
#9365 = CARTESIAN_POINT('',(24.75,0.,45.05)) ;
#9366 = CARTESIAN_POINT('',(24.75,0.,36.15)) ;
#9367 = CARTESIAN_POINT('Origin',(18.5438728059353,0.,45.0908404355877)) ;
#9368 = CARTESIAN_POINT('',(21.2,0.,50.7)) ;
#9369 = CARTESIAN_POINT('',(21.2,0.,50.7)) ;
#9370 = CARTESIAN_POINT('Origin',(18.5438728059353,0.,45.0908404355877)) ;
#9371 = CARTESIAN_POINT('Origin',(0.,0.,8.63269841269837)) ;
#9372 = CARTESIAN_POINT('',(-21.2,0.,50.7)) ;
#9373 = CARTESIAN_POINT('',(-21.2,0.,50.7)) ;
#9374 = CARTESIAN_POINT('Origin',(0.,0.,8.63269841269837)) ;
#9375 = CARTESIAN_POINT('Origin',(-18.2944180372184,0.,44.9341033685178)) ;
#9376 = CARTESIAN_POINT('',(-24.75,0.,45.05)) ;
#9377 = CARTESIAN_POINT('',(-24.75,0.,45.05)) ;
#9378 = CARTESIAN_POINT('Origin',(-18.2944180372184,0.,44.9341033685178)) ;
#9379 = CARTESIAN_POINT('Origin',(-24.75,0.,36.15)) ;
#9380 = CARTESIAN_POINT('',(-24.75,0.,36.15)) ;
#9381 = CARTESIAN_POINT('',(-24.75,0.,36.15)) ;
#9382 = CARTESIAN_POINT('',(-24.75,0.,45.05)) ;
#9383 = CARTESIAN_POINT('Origin',(-24.1,0.,36.15)) ;
#9384 = CARTESIAN_POINT('',(-24.1,0.,35.5)) ;
#9385 = CARTESIAN_POINT('',(-24.1,0.,35.5)) ;
#9386 = CARTESIAN_POINT('Origin',(-24.1,0.,36.15)) ;
#9387 = CARTESIAN_POINT('Origin',(24.1,0.,35.5)) ;
#9388 = CARTESIAN_POINT('',(-6.95,20.65,35.5)) ;
#9389 = CARTESIAN_POINT('',(-9.5,20.65,35.5)) ;
#9390 = CARTESIAN_POINT('',(-6.95,0.,35.5)) ;
#9391 = CARTESIAN_POINT('',(-6.95,7.5,35.5)) ;
#9392 = CARTESIAN_POINT('',(-24.1,0.,35.5)) ;
#9393 = CARTESIAN_POINT('Origin',(-10.,19.79,38.695)) ;
#9394 = CARTESIAN_POINT('',(-6.95,19.79,40.28)) ;
#9395 = CARTESIAN_POINT('',(-10.,19.79,40.28)) ;
#9396 = CARTESIAN_POINT('Origin',(-6.95,19.79,38.695)) ;
#9397 = CARTESIAN_POINT('Origin',(-10.,19.79,38.695)) ;
#9398 = CARTESIAN_POINT('',(6.95,19.79,40.28)) ;
#9399 = CARTESIAN_POINT('Origin',(6.95,19.79,38.695)) ;
#9400 = CARTESIAN_POINT('',(-10.,19.79,40.28)) ;
#9401 = CARTESIAN_POINT('Origin',(6.95,15.,39.2475)) ;
#9402 = CARTESIAN_POINT('',(6.95,0.,45.25)) ;
#9403 = CARTESIAN_POINT('',(6.95,0.,42.43375)) ;
#9404 = CARTESIAN_POINT('',(6.95,20.,45.25)) ;
#9405 = CARTESIAN_POINT('',(6.95,20.,45.25)) ;
#9406 = CARTESIAN_POINT('',(6.95,20.,44.1409526255743)) ;
#9407 = CARTESIAN_POINT('',(6.95,20.,40.3)) ;
#9408 = CARTESIAN_POINT('',(6.95,24.9983082666063,40.3)) ;
#9409 = CARTESIAN_POINT('Origin',(6.95,19.79,38.695)) ;
#9410 = CARTESIAN_POINT('',(6.95,26.2285266168675,40.3)) ;
#9411 = CARTESIAN_POINT('',(6.95,30.,40.3)) ;
#9412 = CARTESIAN_POINT('Origin',(6.95,20.629520265574,41.1654638231566)) ;
#9413 = CARTESIAN_POINT('Origin',(-6.95,20.,45.25)) ;
#9414 = CARTESIAN_POINT('',(-6.95,20.,45.25)) ;
#9415 = CARTESIAN_POINT('',(-6.95,0.,45.25)) ;
#9416 = CARTESIAN_POINT('',(-6.95,20.,45.25)) ;
#9417 = CARTESIAN_POINT('',(-6.95,20.,45.25)) ;
#9418 = CARTESIAN_POINT('',(-3.4749664057175,0.,45.25)) ;
#9419 = CARTESIAN_POINT('Origin',(-6.95,20.,44.1409526255743)) ;
#9420 = CARTESIAN_POINT('',(-6.95,20.,44.1409526255743)) ;
#9421 = CARTESIAN_POINT('',(-6.95,20.,40.3)) ;
#9422 = CARTESIAN_POINT('',(-6.95,20.,44.1409526255743)) ;
#9423 = CARTESIAN_POINT('Origin',(-6.95,19.79,38.695)) ;
#9424 = CARTESIAN_POINT('',(-6.95,24.9983082666063,40.3)) ;
#9425 = CARTESIAN_POINT('Origin',(-6.95,19.79,38.695)) ;
#9426 = CARTESIAN_POINT('',(-6.95,24.9983082666063,40.3)) ;
#9427 = CARTESIAN_POINT('Origin',(-6.95,30.,40.3)) ;
#9428 = CARTESIAN_POINT('',(-6.95,26.2285266168675,40.3)) ;
#9429 = CARTESIAN_POINT('',(-9.5,26.2285266168675,40.3)) ;
#9430 = CARTESIAN_POINT('',(-6.95,30.,40.3)) ;
#9431 = CARTESIAN_POINT('Origin',(-6.95,15.,39.2475)) ;
#9432 = CARTESIAN_POINT('Origin',(-6.95,20.629520265574,41.1654638231566)) ;
#9433 = CARTESIAN_POINT('',(-6.95,0.,42.43375)) ;
#9434 = CARTESIAN_POINT('Origin',(6.71885650094239E-5,0.,45.62)) ;
#9435 = CARTESIAN_POINT('',(19.8,0.,48.29)) ;
#9436 = CARTESIAN_POINT('',(16.75,0.,48.29)) ;
#9437 = CARTESIAN_POINT('Origin',(19.8,0.,45.625)) ;
#9438 = CARTESIAN_POINT('',(-16.75,0.,48.29)) ;
#9439 = CARTESIAN_POINT('',(-19.8,0.,48.29)) ;
#9440 = CARTESIAN_POINT('Origin',(-16.75,0.,45.625)) ;
#9441 = CARTESIAN_POINT('Origin',(-9.5,22.05,46.65)) ;
#9442 = CARTESIAN_POINT('',(-9.5,22.05,46.65)) ;
#9443 = CARTESIAN_POINT('Origin',(-9.5,20.629520265574,41.1654638231566)) ;
#9444 = CARTESIAN_POINT('Origin',(19.8,0.,48.29)) ;
#9445 = CARTESIAN_POINT('',(19.8,0.,48.29)) ;
#9446 = CARTESIAN_POINT('Origin',(19.8,0.,45.625)) ;
#9447 = CARTESIAN_POINT('Origin',(-16.75,0.,48.29)) ;
#9448 = CARTESIAN_POINT('',(-16.75,0.,48.29)) ;
#9449 = CARTESIAN_POINT('Origin',(-16.75,0.,45.625)) ;
#9450 = CARTESIAN_POINT('',(0.,0.,0.)) ;
#9451 = CARTESIAN_POINT('Origin',(-16.5,3.6,5.91295268594296)) ;
#9452 = CARTESIAN_POINT('',(-16.3,3.6,19.9176877660975)) ;
#9453 = CARTESIAN_POINT('',(-16.3,3.6,24.8102001714438)) ;
#9454 = CARTESIAN_POINT('',(-16.3,3.6,5.91295268594296)) ;
#9455 = CARTESIAN_POINT('',(-16.5,3.4,24.8)) ;
#9456 = CARTESIAN_POINT('Ctrl Pts',(-16.3,3.6,24.8102001714438)) ;
#9457 = CARTESIAN_POINT('Ctrl Pts',(-16.3,3.59858329627814,24.8101067420225)) ;
#9458 = CARTESIAN_POINT('Ctrl Pts',(-16.3000150528782,3.59716658347763,24.8100140642958)) ;
#9459 = CARTESIAN_POINT('Ctrl Pts',(-16.3005878505785,3.57021683344479,24.8082647222741)) ;
#9460 = CARTESIAN_POINT('Ctrl Pts',(-16.3060170057452,3.54500851791205,24.8068523074976)) ;
#9461 = CARTESIAN_POINT('Ctrl Pts',(-16.3262650142634,3.49756309113979,24.8043748002524)) ;
#9462 = CARTESIAN_POINT('Ctrl Pts',(-16.3410564019887,3.47584311751711,24.8033431470145)) ;
#9463 = CARTESIAN_POINT('Ctrl Pts',(-16.3781298531838,3.43929965309513,24.801671969686)) ;
#9464 = CARTESIAN_POINT('Ctrl Pts',(-16.4000503702749,3.42482149959621,24.8010487344218)) ;
#9465 = CARTESIAN_POINT('Ctrl Pts',(-16.4482063960532,3.40507852591201,24.8002087457528)) ;
#9466 = CARTESIAN_POINT('Ctrl Pts',(-16.4739783182918,3.4,24.8)) ;
#9467 = CARTESIAN_POINT('Ctrl Pts',(-16.5,3.4,24.8)) ;
#9468 = CARTESIAN_POINT('',(-16.5,3.4,19.9)) ;
#9469 = CARTESIAN_POINT('',(-16.5,3.4,5.91295268594296)) ;
#9470 = CARTESIAN_POINT('Ctrl Pts',(-16.3,3.6,19.9176877660975)) ;
#9471 = CARTESIAN_POINT('Ctrl Pts',(-16.3,3.59869799800569,19.9175543222483)) ;
#9472 = CARTESIAN_POINT('Ctrl Pts',(-16.3000127140685,3.59739597782249,19.9174213564526)) ;
#9473 = CARTESIAN_POINT('Ctrl Pts',(-16.3005412601056,3.57033697971358,19.9146677791384)) ;
#9474 = CARTESIAN_POINT('Ctrl Pts',(-16.3060167422259,3.54489668568216,19.9122633488296)) ;
#9475 = CARTESIAN_POINT('Ctrl Pts',(-16.3264311823542,3.49728852286701,19.9079677236395)) ;
#9476 = CARTESIAN_POINT('Ctrl Pts',(-16.3412454459129,3.47560134784671,19.9061195584593)) ;
#9477 = CARTESIAN_POINT('Ctrl Pts',(-16.3783347386739,3.43915361161839,19.90309493138)) ;
#9478 = CARTESIAN_POINT('Ctrl Pts',(-16.4002305489075,3.42472405685893,19.9019445727726)) ;
#9479 = CARTESIAN_POINT('Ctrl Pts',(-16.4483143342023,3.40505796847904,19.9003903114039)) ;
#9480 = CARTESIAN_POINT('Ctrl Pts',(-16.4740311558542,3.4,19.9)) ;
#9481 = CARTESIAN_POINT('Ctrl Pts',(-16.5,3.4,19.9)) ;
#9482 = CARTESIAN_POINT('Ctrl Pts',(-16.5,3.66900151529807,25.1542076541368)) ;
#9483 = CARTESIAN_POINT('Ctrl Pts',(-16.5,3.36048403150649,25.0953048518056)) ;
#9484 = CARTESIAN_POINT('Ctrl Pts',(-16.5,3.40173214602619,24.7839350218989)) ;
#9485 = CARTESIAN_POINT('Ctrl Pts',(-16.3,3.66900151529807,25.1542076541368)) ;
#9486 = CARTESIAN_POINT('Ctrl Pts',(-16.3,3.36048403150649,25.0953048518056)) ;
#9487 = CARTESIAN_POINT('Ctrl Pts',(-16.3,3.40173214602619,24.7839350218989)) ;
#9488 = CARTESIAN_POINT('Ctrl Pts',(-16.3,3.70650846391527,24.9577560600852)) ;
#9489 = CARTESIAN_POINT('Ctrl Pts',(-16.3,3.58356237630649,24.9342829362712)) ;
#9490 = CARTESIAN_POINT('Ctrl Pts',(-16.3,3.6,24.8102001714438)) ;
#9491 = CARTESIAN_POINT('',(-16.3,3.70650846391527,24.9577560600852)) ;
#9492 = CARTESIAN_POINT('Origin',(-16.3,3.73135783556136,24.8276015460276)) ;
#9493 = CARTESIAN_POINT('',(-16.5,3.65,25.15)) ;
#9494 = CARTESIAN_POINT('Ctrl Pts',(-16.3,3.70650846391514,24.9577560600856)) ;
#9495 = CARTESIAN_POINT('Ctrl Pts',(-16.3,3.70613263983865,24.9591249412769)) ;
#9496 = CARTESIAN_POINT('Ctrl Pts',(-16.3000150182802,3.70575595543002,24.9604935443118)) ;
#9497 = CARTESIAN_POINT('Ctrl Pts',(-16.3005875755283,3.69856163592349,24.9865707375138)) ;
#9498 = CARTESIAN_POINT('Ctrl Pts',(-16.3060248879301,3.69157540066649,25.0108789195648)) ;
#9499 = CARTESIAN_POINT('Ctrl Pts',(-16.3262992686171,3.67823129499146,25.0565205811117)) ;
#9500 = CARTESIAN_POINT('Ctrl Pts',(-16.3410934423138,3.67201058953845,25.0773585750523)) ;
#9501 = CARTESIAN_POINT('Ctrl Pts',(-16.3781678938455,3.66147275373834,25.1123866592332)) ;
#9502 = CARTESIAN_POINT('Ctrl Pts',(-16.4000834311664,3.6572541549447,25.1262472800193)) ;
#9503 = CARTESIAN_POINT('Ctrl Pts',(-16.4482258668633,3.6514907915847,25.1451425855636)) ;
#9504 = CARTESIAN_POINT('Ctrl Pts',(-16.4739878802345,3.64999999999995,25.15)) ;
#9505 = CARTESIAN_POINT('Ctrl Pts',(-16.5,3.64999999999998,25.15)) ;
#9506 = CARTESIAN_POINT('Origin',(-16.5,3.73135783556136,24.8276015460276)) ;
#9507 = CARTESIAN_POINT('Origin',(-16.5,9.21323262385133,26.950665756062)) ;
#9508 = CARTESIAN_POINT('',(-16.3,8.97014939515602,26.862692778058)) ;
#9509 = CARTESIAN_POINT('',(-16.3,9.21323262385133,26.950665756062)) ;
#9510 = CARTESIAN_POINT('',(-16.5,8.9,27.05)) ;
#9511 = CARTESIAN_POINT('Ctrl Pts',(-16.3,8.97014939515603,26.862692778058)) ;
#9512 = CARTESIAN_POINT('Ctrl Pts',(-16.3,8.96980308364479,26.8636177522322)) ;
#9513 = CARTESIAN_POINT('Ctrl Pts',(-16.3000073154306,8.96945677553284,26.8645427132193)) ;
#9514 = CARTESIAN_POINT('Ctrl Pts',(-16.3004060917108,8.96001834123631,26.8897518974964)) ;
#9515 = CARTESIAN_POINT('Ctrl Pts',(-16.3058295041454,8.95103756375146,26.9137357983753)) ;
#9516 = CARTESIAN_POINT('Ctrl Pts',(-16.3261930199806,8.93426601854423,26.9585208446484)) ;
#9517 = CARTESIAN_POINT('Ctrl Pts',(-16.3409790053634,8.92664079883567,26.9788799538846)) ;
#9518 = CARTESIAN_POINT('Ctrl Pts',(-16.3780508878748,8.9138070830345,27.0131430696366)) ;
#9519 = CARTESIAN_POINT('Ctrl Pts',(-16.3999818993935,8.90872114416451,27.0267199513302)) ;
#9520 = CARTESIAN_POINT('Ctrl Pts',(-16.4481661967434,8.90178447987665,27.0452368074562)) ;
#9521 = CARTESIAN_POINT('Ctrl Pts',(-16.4739585659257,8.90000000000001,27.05)) ;
#9522 = CARTESIAN_POINT('Ctrl Pts',(-16.5,8.90000000000002,27.05)) ;
#9523 = CARTESIAN_POINT('',(-16.5,9.14517170941122,27.1387288091202)) ;
#9524 = CARTESIAN_POINT('Origin',(-16.5,6.94557266623349,32.0941410006498)) ;
#9525 = CARTESIAN_POINT('',(-16.3,11.0061123301193,28.223872395635)) ;
#9526 = CARTESIAN_POINT('Origin',(-16.3,6.94557266623349,32.0941410006498)) ;
#9527 = CARTESIAN_POINT('',(-16.5,10.85,28.35)) ;
#9528 = CARTESIAN_POINT('Ctrl Pts',(-16.3,11.0061123301191,28.2238723956351)) ;
#9529 = CARTESIAN_POINT('Ctrl Pts',(-16.3,11.0055804043095,28.224301493411)) ;
#9530 = CARTESIAN_POINT('Ctrl Pts',(-16.3000034791753,11.0050484851111,28.2247305924753)) ;
#9531 = CARTESIAN_POINT('Ctrl Pts',(-16.3002811459799,10.9838233720625,28.2418531493033)) ;
#9532 = CARTESIAN_POINT('Ctrl Pts',(-16.3058150165087,10.9633766729718,28.2583581483241)) ;
#9533 = CARTESIAN_POINT('Ctrl Pts',(-16.326587636426,10.9257047806703,28.2887842809271)) ;
#9534 = CARTESIAN_POINT('Ctrl Pts',(-16.3414529469558,10.9087812480954,28.3024612708628)) ;
#9535 = CARTESIAN_POINT('Ctrl Pts',(-16.3786206798534,10.8803789404869,28.325423504731)) ;
#9536 = CARTESIAN_POINT('Ctrl Pts',(-16.4005420742454,10.8691509765117,28.3345056873288)) ;
#9537 = CARTESIAN_POINT('Ctrl Pts',(-16.448550854448,10.8539092421044,28.3468363151263)) ;
#9538 = CARTESIAN_POINT('Ctrl Pts',(-16.4741508269864,10.85,28.35)) ;
#9539 = CARTESIAN_POINT('Ctrl Pts',(-16.5,10.85,28.35)) ;
#9540 = CARTESIAN_POINT('Origin',(-16.5,6.94557266623349,32.0941410006498)) ;
#9541 = CARTESIAN_POINT('Origin',(-16.5,3.95376271603246,17.8309361222439)) ;
#9542 = CARTESIAN_POINT('',(-16.3,11.9761936845669,29.6534659706104)) ;
#9543 = CARTESIAN_POINT('',(-16.3,3.95376271603246,17.8309361222439)) ;
#9544 = CARTESIAN_POINT('',(-16.5,11.8,29.75)) ;
#9545 = CARTESIAN_POINT('Ctrl Pts',(-16.3,11.9761936845669,29.6534659706104)) ;
#9546 = CARTESIAN_POINT('Ctrl Pts',(-16.3,11.9755977818071,29.6537918503201)) ;
#9547 = CARTESIAN_POINT('Ctrl Pts',(-16.300003428101,11.9750018853708,29.6541177328253)) ;
#9548 = CARTESIAN_POINT('Ctrl Pts',(-16.3002783848306,11.9511052235039,29.6671865363954)) ;
#9549 = CARTESIAN_POINT('Ctrl Pts',(-16.3057856833203,11.9280772247116,29.6797901737401)) ;
#9550 = CARTESIAN_POINT('Ctrl Pts',(-16.3264893687407,11.8855929764578,29.7030577904185)) ;
#9551 = CARTESIAN_POINT('Ctrl Pts',(-16.3413308303542,11.866481196583,29.7135326615679)) ;
#9552 = CARTESIAN_POINT('Ctrl Pts',(-16.3784493831192,11.8344052888093,29.7311205240322)) ;
#9553 = CARTESIAN_POINT('Ctrl Pts',(-16.4003385455048,11.8217190498113,29.7380808841414)) ;
#9554 = CARTESIAN_POINT('Ctrl Pts',(-16.4483848748457,11.8044416410206,29.7475617250063)) ;
#9555 = CARTESIAN_POINT('Ctrl Pts',(-16.4740652235286,11.8,29.75)) ;
#9556 = CARTESIAN_POINT('Ctrl Pts',(-16.5,11.8,29.75)) ;
#9557 = CARTESIAN_POINT('',(-16.5,3.78826756115411,17.9432364059113)) ;
#9558 = CARTESIAN_POINT('Origin',(-16.5,36.5141483124065,16.0157526941183)) ;
#9559 = CARTESIAN_POINT('',(-16.5,23.15,2.55)) ;
#9560 = CARTESIAN_POINT('',(-16.3,23.2911535787711,2.69168913909825)) ;
#9561 = CARTESIAN_POINT('Ctrl Pts',(-16.5,23.15,2.55)) ;
#9562 = CARTESIAN_POINT('Ctrl Pts',(-16.486729830519,23.1500114747416,2.54998861183982)) ;
#9563 = CARTESIAN_POINT('Ctrl Pts',(-16.4734600075965,23.1509563633499,2.55091773409742)) ;
#9564 = CARTESIAN_POINT('Ctrl Pts',(-16.4604518659889,23.1528162761338,2.55276885150634)) ;
#9565 = CARTESIAN_POINT('Ctrl Pts',(-16.4474467031566,23.1546757630104,2.55461954502207)) ;
#9566 = CARTESIAN_POINT('Ctrl Pts',(-16.434703780302,23.1574497571748,2.55739171292631)) ;
#9567 = CARTESIAN_POINT('Ctrl Pts',(-16.4224739412131,23.1610838715948,2.56103056798632)) ;
#9568 = CARTESIAN_POINT('Ctrl Pts',(-16.4102465227141,23.1647172667329,2.56466870282625)) ;
#9569 = CARTESIAN_POINT('Ctrl Pts',(-16.3985326219871,23.1692102516309,2.56917299033804)) ;
#9570 = CARTESIAN_POINT('Ctrl Pts',(-16.3875627358418,23.1744746360492,2.57445458125638)) ;
#9571 = CARTESIAN_POINT('Ctrl Pts',(-16.3765946806012,23.1797381418269,2.57973529066242)) ;
#9572 = CARTESIAN_POINT('Ctrl Pts',(-16.3663709624564,23.1857725150437,2.5857927673833)) ;
#9573 = CARTESIAN_POINT('Ctrl Pts',(-16.3570926888396,23.192459275069,2.59250763886549)) ;
#9574 = CARTESIAN_POINT('Ctrl Pts',(-16.3478091427317,23.1991498349263,2.59922632615453)) ;
#9575 = CARTESIAN_POINT('Ctrl Pts',(-16.3394726039165,23.2064931771287,2.60660280684047)) ;
#9576 = CARTESIAN_POINT('Ctrl Pts',(-16.3322472430606,23.2143449105459,2.61449159764939)) ;
#9577 = CARTESIAN_POINT('Ctrl Pts',(-16.3250249191743,23.222193343716,2.62237707263526)) ;
#9578 = CARTESIAN_POINT('Ctrl Pts',(-16.3189132130904,23.2305493305402,2.63077401379403)) ;
#9579 = CARTESIAN_POINT('Ctrl Pts',(-16.314032381497,23.2392486759751,2.63951697966904)) ;
#9580 = CARTESIAN_POINT('Ctrl Pts',(-16.3091497448563,23.2479512386341,2.6482631789001)) ;
#9581 = CARTESIAN_POINT('Ctrl Pts',(-16.3054991510676,23.2569969611718,2.65735520265509)) ;
#9582 = CARTESIAN_POINT('Ctrl Pts',(-16.3031524836877,23.2662079472228,2.66661380003915)) ;
#9583 = CARTESIAN_POINT('Ctrl Pts',(-16.3010563665765,23.274435489668,2.67488387042443)) ;
#9584 = CARTESIAN_POINT('Ctrl Pts',(-16.3,23.2827944744635,2.6832864252383)) ;
#9585 = CARTESIAN_POINT('Ctrl Pts',(-16.3,23.2911535787711,2.69168913909824)) ;
#9586 = CARTESIAN_POINT('',(-16.3,18.294148957922,11.4980228572171)) ;
#9587 = CARTESIAN_POINT('Origin',(-16.3,36.5141483124065,16.0157526941183)) ;
#9588 = CARTESIAN_POINT('',(-16.5,18.1,11.45)) ;
#9589 = CARTESIAN_POINT('Ctrl Pts',(-16.3,18.2941488864465,11.4980231468811)) ;
#9590 = CARTESIAN_POINT('Ctrl Pts',(-16.3,18.2931711440882,11.4977812986387)) ;
#9591 = CARTESIAN_POINT('Ctrl Pts',(-16.3000076085327,18.2921934151116,11.4975394541029)) ;
#9592 = CARTESIAN_POINT('Ctrl Pts',(-16.3004142507957,18.2660672742078,11.4910770538662)) ;
#9593 = CARTESIAN_POINT('Ctrl Pts',(-16.3058361197429,18.2412305565793,11.4849336180022)) ;
#9594 = CARTESIAN_POINT('Ctrl Pts',(-16.326188866186,18.1948292452181,11.4734561374461)) ;
#9595 = CARTESIAN_POINT('Ctrl Pts',(-16.3409740368393,18.1737258010638,11.4682361612175)) ;
#9596 = CARTESIAN_POINT('Ctrl Pts',(-16.3780452194892,18.1382083382951,11.459450863904)) ;
#9597 = CARTESIAN_POINT('Ctrl Pts',(-16.3999768096068,18.1241338849223,11.4559695344002)) ;
#9598 = CARTESIAN_POINT('Ctrl Pts',(-16.4481630630878,18.1049379542765,11.4512214053032)) ;
#9599 = CARTESIAN_POINT('Ctrl Pts',(-16.4739570389763,18.0999999999998,11.4500000000009)) ;
#9600 = CARTESIAN_POINT('Ctrl Pts',(-16.5,18.0999999999997,11.4500000000014)) ;
#9601 = CARTESIAN_POINT('Origin',(-16.5,36.5141483124065,16.0157526941183)) ;
#9602 = CARTESIAN_POINT('Origin',(-16.5,20.3521649222088,3.15764237037056)) ;
#9603 = CARTESIAN_POINT('',(-16.5,16.2,19.15)) ;
#9604 = CARTESIAN_POINT('',(-16.5,20.1579889903124,3.10972882873379)) ;
#9605 = CARTESIAN_POINT('',(-16.3,16.39481890426,19.1953078115317)) ;
#9606 = CARTESIAN_POINT('',(-16.3,20.3521649222088,3.15764237037056)) ;
#9607 = CARTESIAN_POINT('Ctrl Pts',(-16.3,16.39481890426,19.1953078115317)) ;
#9608 = CARTESIAN_POINT('Ctrl Pts',(-16.3,16.3937985287443,19.1950703246161)) ;
#9609 = CARTESIAN_POINT('Ctrl Pts',(-16.3000082303023,16.3927781683374,19.194832844051)) ;
#9610 = CARTESIAN_POINT('Ctrl Pts',(-16.3004312166973,16.3665596764086,19.1887307763087)) ;
#9611 = CARTESIAN_POINT('Ctrl Pts',(-16.3058537359057,16.3416754708487,19.1829410368996)) ;
#9612 = CARTESIAN_POINT('Ctrl Pts',(-16.3261949626671,16.2951486910566,19.1721187037127)) ;
#9613 = CARTESIAN_POINT('Ctrl Pts',(-16.3409813386088,16.2739730545514,19.1671947135443)) ;
#9614 = CARTESIAN_POINT('Ctrl Pts',(-16.3780535589099,16.2383357459206,19.1589095136144)) ;
#9615 = CARTESIAN_POINT('Ctrl Pts',(-16.399984302301,16.2242141206252,19.1556273129937)) ;
#9616 = CARTESIAN_POINT('Ctrl Pts',(-16.4481676790938,16.2049543635143,19.1511512193477)) ;
#9617 = CARTESIAN_POINT('Ctrl Pts',(-16.4739592878869,16.2,19.15)) ;
#9618 = CARTESIAN_POINT('Ctrl Pts',(-16.5,16.2,19.15)) ;
#9619 = CARTESIAN_POINT('Origin',(-16.5,17.5172318824408,27.2801860892852)) ;
#9620 = CARTESIAN_POINT('',(-16.3,17.1987235045029,33.2996639834704)) ;
#9621 = CARTESIAN_POINT('Origin',(-16.3,17.5172318824408,27.2801860892852)) ;
#9622 = CARTESIAN_POINT('',(-16.5,17.2,33.5)) ;
#9623 = CARTESIAN_POINT('Ctrl Pts',(-16.3,17.1987235045029,33.2996639834704)) ;
#9624 = CARTESIAN_POINT('Ctrl Pts',(-16.3,17.1987232753492,33.3003611800888)) ;
#9625 = CARTESIAN_POINT('Ctrl Pts',(-16.3000036355714,17.1987230858431,33.3010583720144)) ;
#9626 = CARTESIAN_POINT('Ctrl Pts',(-16.3002856442455,17.198717281846,33.328098174988)) ;
#9627 = CARTESIAN_POINT('Ctrl Pts',(-16.3057480719172,17.1987708548077,33.354132367517)) ;
#9628 = CARTESIAN_POINT('Ctrl Pts',(-16.3263180729416,17.1989854907429,33.4023511920969)) ;
#9629 = CARTESIAN_POINT('Ctrl Pts',(-16.3411337274067,17.1991433140337,33.4241154714425)) ;
#9630 = CARTESIAN_POINT('Ctrl Pts',(-16.3782330563044,17.1994835779039,33.4606980218657)) ;
#9631 = CARTESIAN_POINT('Ctrl Pts',(-16.4001489369542,17.1996607382249,33.4751833159373)) ;
#9632 = CARTESIAN_POINT('Ctrl Pts',(-16.448271269925,17.1999215524663,33.494923395259)) ;
#9633 = CARTESIAN_POINT('Ctrl Pts',(-16.474009525343,17.2,33.5)) ;
#9634 = CARTESIAN_POINT('Ctrl Pts',(-16.5,17.2,33.5)) ;
#9635 = CARTESIAN_POINT('Origin',(-16.5,17.5172318824408,27.2801860892852)) ;
#9636 = CARTESIAN_POINT('Origin',(-16.5,27.3698141664511,-1.38697145397653)) ;
#9637 = CARTESIAN_POINT('',(-16.5,35.4,-9.7)) ;
#9638 = CARTESIAN_POINT('',(-16.5,27.2283928102138,-1.52839281021384)) ;
#9639 = CARTESIAN_POINT('',(-16.3,35.5417071354466,-9.55886442297199)) ;
#9640 = CARTESIAN_POINT('Ctrl Pts',(-16.4999999999999,35.4,-9.70000000000001)) ;
#9641 = CARTESIAN_POINT('Ctrl Pts',(-16.4867298305156,35.4000120713885,-9.7000120713885)) ;
#9642 = CARTESIAN_POINT('Ctrl Pts',(-16.4734600075898,35.4009611116237,-9.69908717393026)) ;
#9643 = CARTESIAN_POINT('Ctrl Pts',(-16.4604518659791,35.4028286681215,-9.69724376020955)) ;
#9644 = CARTESIAN_POINT('Ctrl Pts',(-16.4474467031436,35.4046957969616,-9.69540076861792)) ;
#9645 = CARTESIAN_POINT('Ctrl Pts',(-16.434703780286,35.4074809232352,-9.69263977959273)) ;
#9646 = CARTESIAN_POINT('Ctrl Pts',(-16.4224739411945,35.4111294594436,-9.68901538063276)) ;
#9647 = CARTESIAN_POINT('Ctrl Pts',(-16.4102465226927,35.4147772735159,-9.6853916990316)) ;
#9648 = CARTESIAN_POINT('Ctrl Pts',(-16.3985326219634,35.4192879650293,-9.68090513998926)) ;
#9649 = CARTESIAN_POINT('Ctrl Pts',(-16.3875627358162,35.4245730136184,-9.67564422387127)) ;
#9650 = CARTESIAN_POINT('Ctrl Pts',(-16.3765946805737,35.4298571801182,-9.67038418581483)) ;
#9651 = CARTESIAN_POINT('Ctrl Pts',(-16.3663709624275,35.4359151696035,-9.6643503247729)) ;
#9652 = CARTESIAN_POINT('Ctrl Pts',(-16.3570926888101,35.442628054646,-9.65766156817372)) ;
#9653 = CARTESIAN_POINT('Ctrl Pts',(-16.3478091427014,35.4493447543667,-9.65096901060764)) ;
#9654 = CARTESIAN_POINT('Ctrl Pts',(-16.3394726038861,35.4567167467337,-9.6436211603952)) ;
#9655 = CARTESIAN_POINT('Ctrl Pts',(-16.3322472430311,35.4645990935164,-9.63576295576712)) ;
#9656 = CARTESIAN_POINT('Ctrl Pts',(-16.3250249191456,35.4724781271847,-9.627908054106)) ;
#9657 = CARTESIAN_POINT('Ctrl Pts',(-16.3189132130632,35.4808666745071,-9.61954363879068)) ;
#9658 = CARTESIAN_POINT('Ctrl Pts',(-16.3140323814724,35.4895999160555,-9.61083452924953)) ;
#9659 = CARTESIAN_POINT('Ctrl Pts',(-16.3091497448343,35.4983363873636,-9.60212219887312)) ;
#9660 = CARTESIAN_POINT('Ctrl Pts',(-16.3054991510491,35.5074173534341,-9.59306537373435)) ;
#9661 = CARTESIAN_POINT('Ctrl Pts',(-16.3031524836736,35.5166642393525,-9.58384262874775)) ;
#9662 = CARTESIAN_POINT('Ctrl Pts',(-16.3010563665718,35.524923848667,-9.57560458287265)) ;
#9663 = CARTESIAN_POINT('Ctrl Pts',(-16.3,35.5333154223859,-9.56723457259326)) ;
#9664 = CARTESIAN_POINT('Ctrl Pts',(-16.3,35.5417071354465,-9.55886442297206)) ;
#9665 = CARTESIAN_POINT('',(-16.3,27.3698141664511,-1.38697145397653)) ;
#9666 = CARTESIAN_POINT('Origin',(-16.5,17.2261159840305,33.8238840159695)) ;
#9667 = CARTESIAN_POINT('',(-16.3,17.75,33.8570883563426)) ;
#9668 = CARTESIAN_POINT('Origin',(-16.3,17.2261159840305,33.8238840159695)) ;
#9669 = CARTESIAN_POINT('',(-16.5,17.55,33.85)) ;
#9670 = CARTESIAN_POINT('Ctrl Pts',(-16.3,17.7500000000001,33.8570883563426)) ;
#9671 = CARTESIAN_POINT('Ctrl Pts',(-16.3,17.7483048927982,33.8570346913121)) ;
#9672 = CARTESIAN_POINT('Ctrl Pts',(-16.3000215504131,17.7466098579756,33.8569808984551)) ;
#9673 = CARTESIAN_POINT('Ctrl Pts',(-16.3007065293252,17.7196757862025,33.8561240343249)) ;
#9674 = CARTESIAN_POINT('Ctrl Pts',(-16.3061219364636,17.6947845328973,33.8553018126002)) ;
#9675 = CARTESIAN_POINT('Ctrl Pts',(-16.3262385181079,17.6476026569698,33.8536820465369)) ;
#9676 = CARTESIAN_POINT('Ctrl Pts',(-16.3410354339983,17.6258680589014,33.8529014445044)) ;
#9677 = CARTESIAN_POINT('Ctrl Pts',(-16.3781172068274,17.5893078527847,33.8515452810162)) ;
#9678 = CARTESIAN_POINT('Ctrl Pts',(-16.4000425477405,17.5748252688856,33.8509836241205)) ;
#9679 = CARTESIAN_POINT('Ctrl Pts',(-16.4482041298703,17.555078893135,33.8502065060916)) ;
#9680 = CARTESIAN_POINT('Ctrl Pts',(-16.4739769626953,17.55,33.85)) ;
#9681 = CARTESIAN_POINT('Ctrl Pts',(-16.5,17.55,33.85)) ;
#9682 = CARTESIAN_POINT('Origin',(-16.5,17.2261159840305,33.8238840159695)) ;
#9683 = CARTESIAN_POINT('Origin',(-16.5,19.75,10.512952685943)) ;
#9684 = CARTESIAN_POINT('',(-16.5,19.95,37.8)) ;
#9685 = CARTESIAN_POINT('',(-16.3,19.75,37.799163194566)) ;
#9686 = CARTESIAN_POINT('Ctrl Pts',(-16.5,19.95,37.8)) ;
#9687 = CARTESIAN_POINT('Ctrl Pts',(-16.4867298305157,19.95,37.7999646531197)) ;
#9688 = CARTESIAN_POINT('Ctrl Pts',(-16.4734600075899,19.9486749259494,37.7999293062395)) ;
#9689 = CARTESIAN_POINT('Ctrl Pts',(-16.4604518659792,19.9460508737432,37.7998939593592)) ;
#9690 = CARTESIAN_POINT('Ctrl Pts',(-16.4474467031437,19.9434274224269,37.7998586205732)) ;
#9691 = CARTESIAN_POINT('Ctrl Pts',(-16.4347037802861,19.9395057266899,37.7998232817871)) ;
#9692 = CARTESIAN_POINT('Ctrl Pts',(-16.4224739411945,19.9343629849132,37.799787943001)) ;
#9693 = CARTESIAN_POINT('Ctrl Pts',(-16.4102465226928,19.9292212610131,37.7997526112094)) ;
#9694 = CARTESIAN_POINT('Ctrl Pts',(-16.3985326219634,19.9228592441331,37.7997172794177)) ;
#9695 = CARTESIAN_POINT('Ctrl Pts',(-16.3875627358163,19.9154021209746,37.7996819476261)) ;
#9696 = CARTESIAN_POINT('Ctrl Pts',(-16.3765946805737,19.9079462424307,37.7996466217314)) ;
#9697 = CARTESIAN_POINT('Ctrl Pts',(-16.3663709624276,19.8993960129258,37.7996112958368)) ;
#9698 = CARTESIAN_POINT('Ctrl Pts',(-16.3570926888102,19.8899196212419,37.7995759699421)) ;
#9699 = CARTESIAN_POINT('Ctrl Pts',(-16.3478091427015,19.8804378444838,37.7995406239731)) ;
#9700 = CARTESIAN_POINT('Ctrl Pts',(-16.3394726038862,19.8700293439778,37.7995052780041)) ;
#9701 = CARTESIAN_POINT('Ctrl Pts',(-16.3322472430311,19.8588990933357,37.799469932035)) ;
#9702 = CARTESIAN_POINT('Ctrl Pts',(-16.3250249191456,19.8477735209695,37.7994346009226)) ;
#9703 = CARTESIAN_POINT('Ctrl Pts',(-16.3189132130633,19.8359273874834,37.7993992698103)) ;
#9704 = CARTESIAN_POINT('Ctrl Pts',(-16.3140323814724,19.8235937827482,37.7993639386979)) ;
#9705 = CARTESIAN_POINT('Ctrl Pts',(-16.3091497448343,19.8112556167534,37.7993285945192)) ;
#9706 = CARTESIAN_POINT('Ctrl Pts',(-16.3054991510491,19.7984302615936,37.7992932503405)) ;
#9707 = CARTESIAN_POINT('Ctrl Pts',(-16.3031524836737,19.7853702603347,37.7992579061619)) ;
#9708 = CARTESIAN_POINT('Ctrl Pts',(-16.3010563665718,19.7737046564764,37.7992263356299)) ;
#9709 = CARTESIAN_POINT('Ctrl Pts',(-16.3,19.7618524267677,37.799194765098)) ;
#9710 = CARTESIAN_POINT('Ctrl Pts',(-16.3,19.75,37.799163194566)) ;
#9711 = CARTESIAN_POINT('',(-16.3,19.75,33.9947419676036)) ;
#9712 = CARTESIAN_POINT('',(-16.3,19.75,10.512952685943)) ;
#9713 = CARTESIAN_POINT('',(-16.5,19.95,34.)) ;
#9714 = CARTESIAN_POINT('Ctrl Pts',(-16.3,19.75,33.9947419676036)) ;
#9715 = CARTESIAN_POINT('Ctrl Pts',(-16.3,19.7510782785912,33.9947695469051)) ;
#9716 = CARTESIAN_POINT('Ctrl Pts',(-16.3000087201354,19.7521565392984,33.9947971375259)) ;
#9717 = CARTESIAN_POINT('Ctrl Pts',(-16.3002171823642,19.7650440705554,33.9951270456112)) ;
#9718 = CARTESIAN_POINT('Ctrl Pts',(-16.3014539310975,19.7768134007127,33.9954297554171)) ;
#9719 = CARTESIAN_POINT('Ctrl Pts',(-16.3063661361484,19.8019186718149,33.9960784841571)) ;
#9720 = CARTESIAN_POINT('Ctrl Pts',(-16.3103990384751,19.8151237982275,33.9964216349601)) ;
#9721 = CARTESIAN_POINT('Ctrl Pts',(-16.3258880628794,19.8517998580413,33.9973795771215)) ;
#9722 = CARTESIAN_POINT('Ctrl Pts',(-16.3406089202894,19.8735832081072,33.9979548913887)) ;
#9723 = CARTESIAN_POINT('Ctrl Pts',(-16.3775678942223,19.9102753697401,33.9989306239122)) ;
#9724 = CARTESIAN_POINT('Ctrl Pts',(-16.3994500653805,19.9248361652066,33.9993215857928)) ;
#9725 = CARTESIAN_POINT('Ctrl Pts',(-16.4475619545613,19.9447510071692,33.9998577643717)) ;
#9726 = CARTESIAN_POINT('Ctrl Pts',(-16.473330252482,19.9499162250234,33.9999977343853)) ;
#9727 = CARTESIAN_POINT('Ctrl Pts',(-16.4995761386499,19.9499996631663,33.9999999908907)) ;
#9728 = CARTESIAN_POINT('Ctrl Pts',(-16.4997880774491,19.95,34.)) ;
#9729 = CARTESIAN_POINT('Ctrl Pts',(-16.5,19.95,34.)) ;
#9730 = CARTESIAN_POINT('',(-16.5,19.95,10.512952685943)) ;
#9731 = CARTESIAN_POINT('Origin',(-16.5,43.2596418025572,-36.388001295162)) ;
#9732 = CARTESIAN_POINT('',(-16.5,42.3,-58.75)) ;
#9733 = CARTESIAN_POINT('',(-16.5,44.45,-17.3)) ;
#9734 = CARTESIAN_POINT('',(-16.5,43.4593732974275,-36.3983613123869)) ;
#9735 = CARTESIAN_POINT('',(-16.3,44.2502789878669,-17.2894378853552)) ;
#9736 = CARTESIAN_POINT('Ctrl Pts',(-16.5000000000003,44.45,-17.3)) ;
#9737 = CARTESIAN_POINT('Ctrl Pts',(-16.4867298305159,44.4500004427936,-17.2999914633522)) ;
#9738 = CARTESIAN_POINT('Ctrl Pts',(-16.4734600075901,44.4486775904825,-17.2999142877544)) ;
#9739 = CARTESIAN_POINT('Ctrl Pts',(-16.4604518659795,44.4460575039272,-17.2997698249763)) ;
#9740 = CARTESIAN_POINT('Ctrl Pts',(-16.447446703144,44.4434380173538,-17.2996253952791)) ;
#9741 = CARTESIAN_POINT('Ctrl Pts',(-16.4347037802864,44.439522029286,-17.2994137164092)) ;
#9742 = CARTESIAN_POINT('Ctrl Pts',(-16.4224739411948,44.4343866344642,-17.2991387872492)) ;
#9743 = CARTESIAN_POINT('Ctrl Pts',(-16.410246522693,44.429252256065,-17.2988639125046)) ;
#9744 = CARTESIAN_POINT('Ctrl Pts',(-16.3985326219637,44.4228992229604,-17.2985258264785)) ;
#9745 = CARTESIAN_POINT('Ctrl Pts',(-16.3875627358166,44.4154525537855,-17.2981310138529)) ;
#9746 = CARTESIAN_POINT('Ctrl Pts',(-16.376594680574,44.4080071274804,-17.2977362671226)) ;
#9747 = CARTESIAN_POINT('Ctrl Pts',(-16.3663709624278,44.3994688194087,-17.2972848329182)) ;
#9748 = CARTESIAN_POINT('Ctrl Pts',(-16.3570926888104,44.3900055925544,-17.2967854234333)) ;
#9749 = CARTESIAN_POINT('Ctrl Pts',(-16.3478091427017,44.3805369881069,-17.2962857301528)) ;
#9750 = CARTESIAN_POINT('Ctrl Pts',(-16.3394726038863,44.370142904062,-17.2957380325024)) ;
#9751 = CARTESIAN_POINT('Ctrl Pts',(-16.3322472430313,44.3590280388489,-17.2951529481328)) ;
#9752 = CARTESIAN_POINT('Ctrl Pts',(-16.3250249191457,44.3479178454451,-17.2945681096863)) ;
#9753 = CARTESIAN_POINT('Ctrl Pts',(-16.3189132130634,44.336088058293,-17.2939459461117)) ;
#9754 = CARTESIAN_POINT('Ctrl Pts',(-16.3140323814725,44.3237714543345,-17.2932985314845)) ;
#9755 = CARTESIAN_POINT('Ctrl Pts',(-16.3091497448344,44.3114502954038,-17.292650877428)) ;
#9756 = CARTESIAN_POINT('Ctrl Pts',(-16.3054991510492,44.298642601372,-17.2919779869307)) ;
#9757 = CARTESIAN_POINT('Ctrl Pts',(-16.3031524836737,44.2856005762595,-17.2912929417453)) ;
#9758 = CARTESIAN_POINT('Ctrl Pts',(-16.3010563665718,44.2739510292602,-17.2906810378413)) ;
#9759 = CARTESIAN_POINT('Ctrl Pts',(-16.3,44.2621151069607,-17.290059466702)) ;
#9760 = CARTESIAN_POINT('Ctrl Pts',(-16.3,44.2502789878666,-17.2894378853551)) ;
#9761 = CARTESIAN_POINT('',(-16.3,42.1003608836993,-58.737859058676)) ;
#9762 = CARTESIAN_POINT('',(-16.3,43.2596418025572,-36.388001295162)) ;
#9763 = CARTESIAN_POINT('Origin',(-16.5,42.1003608738345,-58.7378592000713)) ;
#9764 = CARTESIAN_POINT('Origin',(-16.5,21.6437725346931,34.0916800205589)) ;
#9765 = CARTESIAN_POINT('',(-16.3,20.6462198057265,32.4790238413936)) ;
#9766 = CARTESIAN_POINT('Origin',(-16.3,21.6437725346931,34.0916800205589)) ;
#9767 = CARTESIAN_POINT('',(-16.5,20.75,32.65)) ;
#9768 = CARTESIAN_POINT('Ctrl Pts',(-16.3,20.6462198057265,32.4790238413936)) ;
#9769 = CARTESIAN_POINT('Ctrl Pts',(-16.3,20.6471046707134,32.4804826685849)) ;
#9770 = CARTESIAN_POINT('Ctrl Pts',(-16.3000218320537,20.6479895107055,32.4819414292721)) ;
#9771 = CARTESIAN_POINT('Ctrl Pts',(-16.3007104860663,20.661942770123,32.5049445855192)) ;
#9772 = CARTESIAN_POINT('Ctrl Pts',(-16.3061131716744,20.67483374418,32.5261907507504)) ;
#9773 = CARTESIAN_POINT('Ctrl Pts',(-16.3261915748286,20.6992980016081,32.5665017177397)) ;
#9774 = CARTESIAN_POINT('Ctrl Pts',(-16.3409772878684,20.7105794706497,32.58508542171)) ;
#9775 = CARTESIAN_POINT('Ctrl Pts',(-16.3780489386812,20.7295683313049,32.6163598571282)) ;
#9776 = CARTESIAN_POINT('Ctrl Pts',(-16.3999801547909,20.737094268172,32.6287518987764)) ;
#9777 = CARTESIAN_POINT('Ctrl Pts',(-16.4481651260864,20.7473591549605,32.6456526692713)) ;
#9778 = CARTESIAN_POINT('Ctrl Pts',(-16.4739580437547,20.75,32.65)) ;
#9779 = CARTESIAN_POINT('Ctrl Pts',(-16.5,20.75,32.65)) ;
#9780 = CARTESIAN_POINT('Origin',(-16.5,21.6437725346931,34.0916800205589)) ;
#9781 = CARTESIAN_POINT('Origin',(-16.5,23.7122919887408,-16.1822567109578)) ;
#9782 = CARTESIAN_POINT('',(-16.5,38.35,-1.45)) ;
#9783 = CARTESIAN_POINT('Origin',(-16.5,23.7122919887408,-16.1822567109578)) ;
#9784 = CARTESIAN_POINT('',(-16.3,38.2088062759988,-1.59164899203244)) ;
#9785 = CARTESIAN_POINT('Ctrl Pts',(-16.5,38.35,-1.45)) ;
#9786 = CARTESIAN_POINT('Ctrl Pts',(-16.4867298305176,38.3499902600277,-1.44999032253691)) ;
#9787 = CARTESIAN_POINT('Ctrl Pts',(-16.4734600075938,38.3490465723702,-1.4509206253905)) ;
#9788 = CARTESIAN_POINT('Ctrl Pts',(-16.4604518659851,38.3471873356328,-1.45277240215352)) ;
#9789 = CARTESIAN_POINT('Ctrl Pts',(-16.4474467031515,38.3453285246479,-1.45462375487236)) ;
#9790 = CARTESIAN_POINT('Ctrl Pts',(-16.4347037802957,38.3425546817605,-1.45739606102526)) ;
#9791 = CARTESIAN_POINT('Ctrl Pts',(-16.4224739412057,38.3389202236103,-1.46103456278714)) ;
#9792 = CARTESIAN_POINT('Ctrl Pts',(-16.4102465227056,38.33528648481,-1.46467234439889)) ;
#9793 = CARTESIAN_POINT('Ctrl Pts',(-16.3985326219777,38.3307926615411,-1.46917578743196)) ;
#9794 = CARTESIAN_POINT('Ctrl Pts',(-16.3875627358317,38.3255269931887,-1.47445609142917)) ;
#9795 = CARTESIAN_POINT('Ctrl Pts',(-16.3765946805903,38.320262203691,-1.4797355141289)) ;
#9796 = CARTESIAN_POINT('Ctrl Pts',(-16.3663709624449,38.3142261014913,-1.48579126199939)) ;
#9797 = CARTESIAN_POINT('Ctrl Pts',(-16.3570926888279,38.3075372339825,-1.49250402878747)) ;
#9798 = CARTESIAN_POINT('Ctrl Pts',(-16.3478091427197,38.3008445654438,-1.49922061018643)) ;
#9799 = CARTESIAN_POINT('Ctrl Pts',(-16.3394726039044,38.2934987358228,-1.5065946089037)) ;
#9800 = CARTESIAN_POINT('Ctrl Pts',(-16.3322472430489,38.2856442181935,-1.51448062303995)) ;
#9801 = CARTESIAN_POINT('Ctrl Pts',(-16.3250249191629,38.2777930019814,-1.52236332252028)) ;
#9802 = CARTESIAN_POINT('Ctrl Pts',(-16.3189132130796,38.2694339358032,-1.53075719394756)) ;
#9803 = CARTESIAN_POINT('Ctrl Pts',(-16.3140323814872,38.2607313083892,-1.5394968888988)) ;
#9804 = CARTESIAN_POINT('Ctrl Pts',(-16.3091497448476,38.2520254625372,-1.54823981599646)) ;
#9805 = CARTESIAN_POINT('Ctrl Pts',(-16.3054991510602,38.2429762542893,-1.55732836653302)) ;
#9806 = CARTESIAN_POINT('Ctrl Pts',(-16.3031524836821,38.233761681978,-1.56658339086779)) ;
#9807 = CARTESIAN_POINT('Ctrl Pts',(-16.3010563665746,38.2255309361809,-1.57485026968463)) ;
#9808 = CARTESIAN_POINT('Ctrl Pts',(-16.3,38.2171686680524,-1.58324955352066)) ;
#9809 = CARTESIAN_POINT('Ctrl Pts',(-16.3,38.2088062759988,-1.59164899203244)) ;
#9810 = CARTESIAN_POINT('Origin',(-16.3,23.7122919887408,-16.1822567109578)) ;
#9811 = CARTESIAN_POINT('Origin',(-16.5,17.453364864871,27.1098816953352)) ;
#9812 = CARTESIAN_POINT('',(-16.3,23.7,27.1493776981789)) ;
#9813 = CARTESIAN_POINT('Origin',(-16.3,17.453364864871,27.1098816953352)) ;
#9814 = CARTESIAN_POINT('',(-16.5,23.9,27.15)) ;
#9815 = CARTESIAN_POINT('Ctrl Pts',(-16.3,23.7000000155168,27.1493727892874)) ;
#9816 = CARTESIAN_POINT('Ctrl Pts',(-16.3000000001223,23.701576033318,27.1493777710131)) ;
#9817 = CARTESIAN_POINT('Ctrl Pts',(-16.300018628741,23.7031519805708,27.1493827515887)) ;
#9818 = CARTESIAN_POINT('Ctrl Pts',(-16.3006547601165,23.7300560874974,27.1494677621026)) ;
#9819 = CARTESIAN_POINT('Ctrl Pts',(-16.3060610729129,23.7550416808744,27.1495464596783)) ;
#9820 = CARTESIAN_POINT('Ctrl Pts',(-16.3261891818602,23.8023134117509,27.1496949552357)) ;
#9821 = CARTESIAN_POINT('Ctrl Pts',(-16.3409744121654,23.8240528090639,27.1497630282075)) ;
#9822 = CARTESIAN_POINT('Ctrl Pts',(-16.3780456454816,23.8606404855451,27.149877384696)) ;
#9823 = CARTESIAN_POINT('Ctrl Pts',(-16.3999771910801,23.8751390022259,27.1499225811532)) ;
#9824 = CARTESIAN_POINT('Ctrl Pts',(-16.4481632972522,23.8949132761296,27.1499841811634)) ;
#9825 = CARTESIAN_POINT('Ctrl Pts',(-16.4739571531563,23.9,27.15)) ;
#9826 = CARTESIAN_POINT('Ctrl Pts',(-16.5,23.9,27.15)) ;
#9827 = CARTESIAN_POINT('Origin',(-16.5,17.453364864871,27.1098816953352)) ;
#9828 = CARTESIAN_POINT('Origin',(-16.5,33.4726637867458,16.9651420152427)) ;
#9829 = CARTESIAN_POINT('',(-16.5,23.9,16.95)) ;
#9830 = CARTESIAN_POINT('',(-16.3,23.7000000012803,16.9498418202582)) ;
#9831 = CARTESIAN_POINT('Ctrl Pts',(-16.5,23.9,16.95)) ;
#9832 = CARTESIAN_POINT('Ctrl Pts',(-16.4867298305178,23.8999999896474,16.950006544798)) ;
#9833 = CARTESIAN_POINT('Ctrl Pts',(-16.4734600075941,23.8986749069092,16.9500109936177)) ;
#9834 = CARTESIAN_POINT('Ctrl Pts',(-16.4604518659855,23.8960508476347,16.950013395784)) ;
#9835 = CARTESIAN_POINT('Ctrl Pts',(-16.447446703152,23.8934273892517,16.9500157974002)) ;
#9836 = CARTESIAN_POINT('Ctrl Pts',(-16.4347037802963,23.8895056880666,16.9500161535546)) ;
#9837 = CARTESIAN_POINT('Ctrl Pts',(-16.4224739412065,23.8843629423518,16.9500145938707)) ;
#9838 = CARTESIAN_POINT('Ctrl Pts',(-16.4102465227065,23.8792212145144,16.9500130344956)) ;
#9839 = CARTESIAN_POINT('Ctrl Pts',(-16.3985326219787,23.8728591952062,16.9500095604991)) ;
#9840 = CARTESIAN_POINT('Ctrl Pts',(-16.3875627358327,23.8654020709616,16.9500043763796)) ;
#9841 = CARTESIAN_POINT('Ctrl Pts',(-16.3765946805914,23.8579461913319,16.9499991931253)) ;
#9842 = CARTESIAN_POINT('Ctrl Pts',(-16.3663709624461,23.8493959620825,16.9499923009626)) ;
#9843 = CARTESIAN_POINT('Ctrl Pts',(-16.3570926888291,23.839919571777,16.9499839709371)) ;
#9844 = CARTESIAN_POINT('Ctrl Pts',(-16.347809142721,23.8304377963981,16.9499756361781)) ;
#9845 = CARTESIAN_POINT('Ctrl Pts',(-16.3394726039057,23.820029298395,16.9499658627199)) ;
#9846 = CARTESIAN_POINT('Ctrl Pts',(-16.3322472430501,23.8088990511176,16.9499549779694)) ;
#9847 = CARTESIAN_POINT('Ctrl Pts',(-16.3250249191641,23.797773482115,16.9499440977939)) ;
#9848 = CARTESIAN_POINT('Ctrl Pts',(-16.3189132130807,23.7859273528529,16.9499321081945)) ;
#9849 = CARTESIAN_POINT('Ctrl Pts',(-16.3140323814882,23.7735937529089,16.949919378958)) ;
#9850 = CARTESIAN_POINT('Ctrl Pts',(-16.3091497448485,23.7612555917073,16.9499066450139)) ;
#9851 = CARTESIAN_POINT('Ctrl Pts',(-16.305499151061,23.7484302419074,16.9498931719074)) ;
#9852 = CARTESIAN_POINT('Ctrl Pts',(-16.3031524836827,23.735370246261,16.9498793579648)) ;
#9853 = CARTESIAN_POINT('Ctrl Pts',(-16.3010563665748,23.7237046473967,16.9498670189167)) ;
#9854 = CARTESIAN_POINT('Ctrl Pts',(-16.3,23.7118524228822,16.9498544088282)) ;
#9855 = CARTESIAN_POINT('Ctrl Pts',(-16.3,23.7000000012803,16.9498418202582)) ;
#9856 = CARTESIAN_POINT('',(-16.3,26.5585000901577,10.0586572410252)) ;
#9857 = CARTESIAN_POINT('Origin',(-16.3,33.4726637867458,16.9651420152427)) ;
#9858 = CARTESIAN_POINT('',(-16.5,26.7,10.2)) ;
#9859 = CARTESIAN_POINT('Origin',(-16.5,26.5585000901577,10.0586572410252)) ;
#9860 = CARTESIAN_POINT('Origin',(-16.5,33.4726637867458,16.9651420152427)) ;
#9861 = CARTESIAN_POINT('Origin',(-16.5,23.7,1.98795268594296)) ;
#9862 = CARTESIAN_POINT('',(-16.3,23.7,1.98795268594296)) ;
#9863 = CARTESIAN_POINT('',(-16.5,23.9,1.98795268594296)) ;
#9864 = CARTESIAN_POINT('Origin',(-16.5,37.4869714539765,-0.869814166451151)) ;
#9865 = CARTESIAN_POINT('',(-16.5,37.6283928102138,-0.72839281021384)) ;
#9866 = CARTESIAN_POINT('',(-16.3,37.4869714539765,-0.869814166451151)) ;
#9867 = CARTESIAN_POINT('Origin',(-16.5,43.5701155187154,-37.6713759567788)) ;
#9868 = CARTESIAN_POINT('',(-16.5,42.15,-60.9)) ;
#9869 = CARTESIAN_POINT('',(-16.5,43.7696305388826,-37.6852956093486)) ;
#9870 = CARTESIAN_POINT('',(-16.3,41.9506268879594,-60.8840463309467)) ;
#9871 = CARTESIAN_POINT('',(-16.3,43.5701155187154,-37.6713759567788)) ;
#9872 = CARTESIAN_POINT('Ctrl Pts',(-16.3,41.9506268879594,-60.8840463309467)) ;
#9873 = CARTESIAN_POINT('Ctrl Pts',(-16.3,41.9517471911502,-60.8841361107774)) ;
#9874 = CARTESIAN_POINT('Ctrl Pts',(-16.3000094725398,41.9528674746344,-60.8842258867201)) ;
#9875 = CARTESIAN_POINT('Ctrl Pts',(-16.3004632147513,41.9796968069122,-60.8863758482814)) ;
#9876 = CARTESIAN_POINT('Ctrl Pts',(-16.3058831665225,42.0050812395992,-60.8884087660428)) ;
#9877 = CARTESIAN_POINT('Ctrl Pts',(-16.3261922917654,42.0526243758533,-60.8922143172951)) ;
#9878 = CARTESIAN_POINT('Ctrl Pts',(-16.3409781044896,42.074295218724,-60.893947902738)) ;
#9879 = CARTESIAN_POINT('Ctrl Pts',(-16.3780498309033,42.1107665799089,-60.8968644715331)) ;
#9880 = CARTESIAN_POINT('Ctrl Pts',(-16.3999809367931,42.1252187814051,-60.8980196294309)) ;
#9881 = CARTESIAN_POINT('Ctrl Pts',(-16.4481655949025,42.1449296139692,-60.8995949062458)) ;
#9882 = CARTESIAN_POINT('Ctrl Pts',(-16.4739582736902,42.15,-60.8999999999999)) ;
#9883 = CARTESIAN_POINT('Ctrl Pts',(-16.5,42.1500000000001,-60.8999999999991)) ;
#9884 = CARTESIAN_POINT('Origin',(-16.5,18.75,37.7899579831933)) ;
#9885 = CARTESIAN_POINT('',(-16.5,17.55,37.8)) ;
#9886 = CARTESIAN_POINT('',(-16.3,17.7500003499425,37.7991631591148)) ;
#9887 = CARTESIAN_POINT('Ctrl Pts',(-16.5,17.55,37.8)) ;
#9888 = CARTESIAN_POINT('Ctrl Pts',(-16.4867298362033,17.5500003549376,37.8000424142976)) ;
#9889 = CARTESIAN_POINT('Ctrl Pts',(-16.4734600189644,17.55132573864,37.8000737393719)) ;
#9890 = CARTESIAN_POINT('Ctrl Pts',(-16.4604518827053,17.5539500526455,37.8000937776279)) ;
#9891 = CARTESIAN_POINT('Ctrl Pts',(-16.4474467253984,17.5565737656652,37.8001138112951)) ;
#9892 = CARTESIAN_POINT('Ctrl Pts',(-16.4347038077254,17.5604956752289,37.8001225626839)) ;
#9893 = CARTESIAN_POINT('Ctrl Pts',(-16.4224739731519,17.5656385824154,37.8001202894756)) ;
#9894 = CARTESIAN_POINT('Ctrl Pts',(-16.4102465594111,17.57078047159,37.8001180167172)) ;
#9895 = CARTESIAN_POINT('Ctrl Pts',(-16.3985326627544,17.5771426052934,37.8001047243444)) ;
#9896 = CARTESIAN_POINT('Ctrl Pts',(-16.3875627796997,17.584599798429,37.8000811250022)) ;
#9897 = CARTESIAN_POINT('Ctrl Pts',(-16.3765947278103,17.5920557467608,37.8000575295993)) ;
#9898 = CARTESIAN_POINT('Ctrl Pts',(-16.3663710120005,17.600605999172,37.8000236325339)) ;
#9899 = CARTESIAN_POINT('Ctrl Pts',(-16.3570927394624,17.6100823706619,37.7999805824503)) ;
#9900 = CARTESIAN_POINT('Ctrl Pts',(-16.3478091947644,17.6195641268768,37.7999375079045)) ;
#9901 = CARTESIAN_POINT('Ctrl Pts',(-16.3394726560326,17.6299725636313,37.7998852729588)) ;
#9902 = CARTESIAN_POINT('Ctrl Pts',(-16.3322472937619,17.6411027132277,37.7998254284371)) ;
#9903 = CARTESIAN_POINT('Ctrl Pts',(-16.3250249685983,17.6522281843796,37.7997656090704)) ;
#9904 = CARTESIAN_POINT('Ctrl Pts',(-16.3189132596971,17.6640741793753,37.7996981907095)) ;
#9905 = CARTESIAN_POINT('Ctrl Pts',(-16.3140324236727,17.6764076162048,37.7996250677075)) ;
#9906 = CARTESIAN_POINT('Ctrl Pts',(-16.3091497826833,17.6887456140198,37.7995519176641)) ;
#9907 = CARTESIAN_POINT('Ctrl Pts',(-16.3054991828882,17.7015707715661,37.7994730638621)) ;
#9908 = CARTESIAN_POINT('Ctrl Pts',(-16.3031525078829,17.7146305553493,37.7993906788029)) ;
#9909 = CARTESIAN_POINT('Ctrl Pts',(-16.3010563747267,17.7262960163692,37.7993170895528)) ;
#9910 = CARTESIAN_POINT('Ctrl Pts',(-16.3,17.7381480890742,37.7992406894262)) ;
#9911 = CARTESIAN_POINT('Ctrl Pts',(-16.3,17.7500003499425,37.7991631591148)) ;
#9912 = CARTESIAN_POINT('Origin',(-16.3,18.75,37.7899579831933)) ;
#9913 = CARTESIAN_POINT('Origin',(-16.5,18.75,37.7899579831933)) ;
#9914 = CARTESIAN_POINT('Origin',(-16.5,37.7318176617063,-60.502128268216)) ;
#9915 = CARTESIAN_POINT('',(-16.5,36.65,-56.2)) ;
#9916 = CARTESIAN_POINT('Origin',(-16.5,37.7318176617063,-60.502128268216)) ;
#9917 = CARTESIAN_POINT('',(-16.3,36.8459456848986,-56.3597323992937)) ;
#9918 = CARTESIAN_POINT('Origin',(-16.3,37.7318176617063,-60.502128268216)) ;
#9919 = CARTESIAN_POINT('Ctrl Pts',(-16.3,36.8459456848986,-56.3597323992937)) ;
#9920 = CARTESIAN_POINT('Ctrl Pts',(-16.3,36.8452932432187,-56.3591906677183)) ;
#9921 = CARTESIAN_POINT('Ctrl Pts',(-16.3000033286272,36.8446407490739,-56.3586489949852)) ;
#9922 = CARTESIAN_POINT('Ctrl Pts',(-16.3001926160016,36.8260916784102,-56.3432532583223)) ;
#9923 = CARTESIAN_POINT('Ctrl Pts',(-16.3028806855463,36.8081301664174,-56.328423604229)) ;
#9924 = CARTESIAN_POINT('Ctrl Pts',(-16.3132358643299,36.7736693811157,-56.3001110660322)) ;
#9925 = CARTESIAN_POINT('Ctrl Pts',(-16.3207681279902,36.7570768798036,-56.2865472202179)) ;
#9926 = CARTESIAN_POINT('Ctrl Pts',(-16.3435477982502,36.7216811428078,-56.2577328860845)) ;
#9927 = CARTESIAN_POINT('Ctrl Pts',(-16.3603327562665,36.7034378018957,-56.2429732328781)) ;
#9928 = CARTESIAN_POINT('Ctrl Pts',(-16.3980903936837,36.6760935350204,-56.220928962173)) ;
#9929 = CARTESIAN_POINT('Ctrl Pts',(-16.417515115282,36.6660883821569,-56.2128959810192)) ;
#9930 = CARTESIAN_POINT('Ctrl Pts',(-16.4584357635178,36.653234532305,-56.2025876834372)) ;
#9931 = CARTESIAN_POINT('Ctrl Pts',(-16.4790164237796,36.65,-56.2)) ;
#9932 = CARTESIAN_POINT('Ctrl Pts',(-16.5,36.65,-56.2)) ;
#9933 = CARTESIAN_POINT('Origin',(-16.5,17.75,12.412952685943)) ;
#9934 = CARTESIAN_POINT('',(-16.3,17.75,12.412952685943)) ;
#9935 = CARTESIAN_POINT('',(-16.5,17.55,12.412952685943)) ;
#9936 = CARTESIAN_POINT('Origin',(-16.5,29.7633733578399,-15.291248496029)) ;
#9937 = CARTESIAN_POINT('',(-16.5,37.7,-15.5)) ;
#9938 = CARTESIAN_POINT('Origin',(-16.5,29.7633733578399,-15.291248496029)) ;
#9939 = CARTESIAN_POINT('',(-16.3,37.8999308547965,-15.5052586405422)) ;
#9940 = CARTESIAN_POINT('Origin',(-16.5,37.8999308547965,-15.5052586405422)) ;
#9941 = CARTESIAN_POINT('Origin',(-16.3,29.7633733578399,-15.291248496029)) ;
#9942 = CARTESIAN_POINT('Origin',(-16.5,37.9279179147939,-14.4204278690655)) ;
#9943 = CARTESIAN_POINT('',(-16.3,37.9279179147939,-14.4204278690655)) ;
#9944 = CARTESIAN_POINT('',(-16.5,37.7279844379825,-14.415269880106)) ;
#9945 = CARTESIAN_POINT('Origin',(-16.5,12.5256959686759,18.3486581187154)) ;
#9946 = CARTESIAN_POINT('',(-16.5,15.5,20.65)) ;
#9947 = CARTESIAN_POINT('Origin',(-16.5,12.5256959686759,18.3486581187154)) ;
#9948 = CARTESIAN_POINT('',(-16.3,15.63399980594,20.8033220974013)) ;
#9949 = CARTESIAN_POINT('Origin',(-16.3,12.5256959686759,18.3486581187154)) ;
#9950 = CARTESIAN_POINT('Ctrl Pts',(-16.3,15.63399980594,20.8033220974013)) ;
#9951 = CARTESIAN_POINT('Ctrl Pts',(-16.3,15.6335509952834,20.8028060276236)) ;
#9952 = CARTESIAN_POINT('Ctrl Pts',(-16.3000033875055,15.633102174688,20.8022899714548)) ;
#9953 = CARTESIAN_POINT('Ctrl Pts',(-16.300280172625,15.6147658776647,20.7812078286703)) ;
#9954 = CARTESIAN_POINT('Ctrl Pts',(-16.3059282130228,15.5970507182787,20.7608811682357)) ;
#9955 = CARTESIAN_POINT('Ctrl Pts',(-16.3270273887872,15.5646346653857,20.7237524476597)) ;
#9956 = CARTESIAN_POINT('Ctrl Pts',(-16.341968842749,15.5501345809321,20.7071773901075)) ;
#9957 = CARTESIAN_POINT('Ctrl Pts',(-16.3791047732673,15.5259533953226,20.6795690847363)) ;
#9958 = CARTESIAN_POINT('Ctrl Pts',(-16.4008132433006,15.5164134390286,20.6686952926497)) ;
#9959 = CARTESIAN_POINT('Ctrl Pts',(-16.448352927527,15.5034318834199,20.6539056000502)) ;
#9960 = CARTESIAN_POINT('Ctrl Pts',(-16.4736593458904,15.500064924654,20.6500739112853)) ;
#9961 = CARTESIAN_POINT('Ctrl Pts',(-16.4995041564433,15.5000003098668,20.6500003527573)) ;
#9962 = CARTESIAN_POINT('Ctrl Pts',(-16.4997520907635,15.5,20.65)) ;
#9963 = CARTESIAN_POINT('Ctrl Pts',(-16.5,15.5,20.65)) ;
#9964 = CARTESIAN_POINT('Origin',(-16.5,24.7469152941988,15.4731262457782)) ;
#9965 = CARTESIAN_POINT('',(-16.5,12.85,22.2)) ;
#9966 = CARTESIAN_POINT('',(-16.5,24.6459386311912,15.3004887251523)) ;
#9967 = CARTESIAN_POINT('',(-16.3,12.9183976933795,22.3916931443706)) ;
#9968 = CARTESIAN_POINT('',(-16.3,24.7469152941988,15.4731262457782)) ;
#9969 = CARTESIAN_POINT('Ctrl Pts',(-16.3,12.9183976933795,22.3916931443706)) ;
#9970 = CARTESIAN_POINT('Ctrl Pts',(-16.3,12.9181668378952,22.3910505718131)) ;
#9971 = CARTESIAN_POINT('Ctrl Pts',(-16.3000033789794,12.9179359974519,22.3904079978298)) ;
#9972 = CARTESIAN_POINT('Ctrl Pts',(-16.30027972266,12.9084972701201,22.3641323186868)) ;
#9973 = CARTESIAN_POINT('Ctrl Pts',(-16.3059239690591,12.8994116223236,22.3387679571224)) ;
#9974 = CARTESIAN_POINT('Ctrl Pts',(-16.3270129833413,12.8828359249044,22.2923792487433)) ;
#9975 = CARTESIAN_POINT('Ctrl Pts',(-16.3419513881418,12.8754470934585,22.2716433563484)) ;
#9976 = CARTESIAN_POINT('Ctrl Pts',(-16.3790879803581,12.8631486026243,22.2370711958976)) ;
#9977 = CARTESIAN_POINT('Ctrl Pts',(-16.4008036126822,12.8583107467619,22.2234396941227)) ;
#9978 = CARTESIAN_POINT('Ctrl Pts',(-16.4483630640904,12.8517330735393,22.2048939197986)) ;
#9979 = CARTESIAN_POINT('Ctrl Pts',(-16.4736838335087,12.8500311854431,22.2000880211873)) ;
#9980 = CARTESIAN_POINT('Ctrl Pts',(-16.4995289737795,12.8500001414228,22.2000003991673)) ;
#9981 = CARTESIAN_POINT('Ctrl Pts',(-16.4997644981787,12.85,22.2)) ;
#9982 = CARTESIAN_POINT('Ctrl Pts',(-16.5,12.85,22.2)) ;
#9983 = CARTESIAN_POINT('Origin',(-16.5,12.2182755082439,18.0689260404997)) ;
#9984 = CARTESIAN_POINT('',(-16.3,10.7319977197221,22.1880843115736)) ;
#9985 = CARTESIAN_POINT('Origin',(-16.3,12.2182755082439,18.0689260404997)) ;
#9986 = CARTESIAN_POINT('',(-16.5,10.8,22.)) ;
#9987 = CARTESIAN_POINT('Ctrl Pts',(-16.3,10.7319962300621,22.188083771842)) ;
#9988 = CARTESIAN_POINT('Ctrl Pts',(-16.3,10.7325345967251,22.1865948017166)) ;
#9989 = CARTESIAN_POINT('Ctrl Pts',(-16.3000188015201,10.7330729440135,22.1851058840645)) ;
#9990 = CARTESIAN_POINT('Ctrl Pts',(-16.3006567864184,10.7422054211292,22.1598480046429)) ;
#9991 = CARTESIAN_POINT('Ctrl Pts',(-16.306044429893,10.7506834755747,22.1363998527687)) ;
#9992 = CARTESIAN_POINT('Ctrl Pts',(-16.3261195505325,10.7667448574687,22.0919777741593)) ;
#9993 = CARTESIAN_POINT('Ctrl Pts',(-16.3408899811084,10.7741400552678,22.0715241613828)) ;
#9994 = CARTESIAN_POINT('Ctrl Pts',(-16.3779363523888,10.7865890441552,22.0370925871774)) ;
#9995 = CARTESIAN_POINT('Ctrl Pts',(-16.3998581079217,10.7915238186497,22.0234438094466)) ;
#9996 = CARTESIAN_POINT('Ctrl Pts',(-16.4480309426183,10.798258479926,22.0048167970752)) ;
#9997 = CARTESIAN_POINT('Ctrl Pts',(-16.4738214623161,10.7999939814404,22.0000166464488)) ;
#9998 = CARTESIAN_POINT('Ctrl Pts',(-16.4999096104036,10.7999999947913,22.0000000144066)) ;
#9999 = CARTESIAN_POINT('Ctrl Pts',(-16.4999548051947,10.8,22.)) ;
#10000 = CARTESIAN_POINT('Ctrl Pts',(-16.5,10.8,22.)) ;
#10001 = CARTESIAN_POINT('Origin',(-16.5,12.2182755082439,18.0689260404997)) ;
#10002 = CARTESIAN_POINT('Origin',(-16.5,7.48858533183141,21.0129348956712)) ;
#10003 = CARTESIAN_POINT('',(-16.5,3.9,19.5)) ;
#10004 = CARTESIAN_POINT('',(-16.5,7.5567150872414,20.8248967707396)) ;
#10005 = CARTESIAN_POINT('',(-16.3,3.86223646644424,19.6990403792266)) ;
#10006 = CARTESIAN_POINT('',(-16.3,7.48858533183141,21.0129348956712)) ;
#10007 = CARTESIAN_POINT('Ctrl Pts',(-16.3,3.86223646644424,19.6990403792266)) ;
#10008 = CARTESIAN_POINT('Ctrl Pts',(-16.3,3.86239942575251,19.6980436824249)) ;
#10009 = CARTESIAN_POINT('Ctrl Pts',(-16.3000073893637,3.86256289052269,19.6970470816371)) ;
#10010 = CARTESIAN_POINT('Ctrl Pts',(-16.300415494326,3.86708910313053,19.6695382704772)) ;
#10011 = CARTESIAN_POINT('Ctrl Pts',(-16.3060387827755,3.87175164288346,19.6434145527853)) ;
#10012 = CARTESIAN_POINT('Ctrl Pts',(-16.3269910238586,3.88069316641222,19.595511341096)) ;
#10013 = CARTESIAN_POINT('Ctrl Pts',(-16.3418706315149,3.88489021711546,19.5740942364014)) ;
#10014 = CARTESIAN_POINT('Ctrl Pts',(-16.3789985932666,3.8920605693635,19.5382677000811)) ;
#10015 = CARTESIAN_POINT('Ctrl Pts',(-16.4008118680422,3.89497313876539,19.5241432650165)) ;
#10016 = CARTESIAN_POINT('Ctrl Pts',(-16.4486601696573,3.89895928341784,19.5049329178167)) ;
#10017 = CARTESIAN_POINT('Ctrl Pts',(-16.4742006804809,3.9,19.5)) ;
#10018 = CARTESIAN_POINT('Ctrl Pts',(-16.5,3.9,19.5)) ;
#10019 = CARTESIAN_POINT('Origin',(-16.5,3.86867726849999,19.973346585625)) ;
#10020 = CARTESIAN_POINT('Origin',(-16.5,3.86867726849999,19.973346585625)) ;
#10021 = CARTESIAN_POINT('Origin',(-16.3,3.86867726849999,19.973346585625)) ;
#10022 = CARTESIAN_POINT('Origin',(-24.25,3.86867726849999,19.973346585625)) ;
#10023 = CARTESIAN_POINT('',(-24.05,3.4,19.9)) ;
#10024 = CARTESIAN_POINT('',(-24.25,3.4,19.9)) ;
#10025 = CARTESIAN_POINT('',(-24.05,3.9,19.5)) ;
#10026 = CARTESIAN_POINT('Origin',(-24.05,3.86867726849999,19.973346585625)) ;
#10027 = CARTESIAN_POINT('',(-24.25,3.9,19.5)) ;
#10028 = CARTESIAN_POINT('Origin',(-24.25,3.4,24.8)) ;
#10029 = CARTESIAN_POINT('',(-24.05,3.4,24.8)) ;
#10030 = CARTESIAN_POINT('',(-24.25,3.4,24.8)) ;
#10031 = CARTESIAN_POINT('',(-24.05,3.4,5.91295268594296)) ;
#10032 = CARTESIAN_POINT('Origin',(-24.25,3.73135783556136,24.8276015460276)) ;
#10033 = CARTESIAN_POINT('',(-24.05,3.65,25.15)) ;
#10034 = CARTESIAN_POINT('',(-24.25,3.65,25.15)) ;
#10035 = CARTESIAN_POINT('Origin',(-24.05,3.73135783556136,24.8276015460276)) ;
#10036 = CARTESIAN_POINT('Origin',(-24.25,8.9,27.05)) ;
#10037 = CARTESIAN_POINT('',(-24.05,8.9,27.05)) ;
#10038 = CARTESIAN_POINT('',(-24.25,8.9,27.05)) ;
#10039 = CARTESIAN_POINT('',(-24.05,9.14517170941122,27.1387288091202)) ;
#10040 = CARTESIAN_POINT('Origin',(-24.25,6.94557266623349,32.0941410006498)) ;
#10041 = CARTESIAN_POINT('',(-24.05,10.85,28.35)) ;
#10042 = CARTESIAN_POINT('',(-24.25,10.85,28.35)) ;
#10043 = CARTESIAN_POINT('Origin',(-24.05,6.94557266623349,32.0941410006498)) ;
#10044 = CARTESIAN_POINT('Origin',(-24.25,11.8,29.75)) ;
#10045 = CARTESIAN_POINT('',(-24.05,11.8,29.75)) ;
#10046 = CARTESIAN_POINT('',(-24.25,11.8,29.75)) ;
#10047 = CARTESIAN_POINT('',(-24.05,3.78826756115411,17.9432364059113)) ;
#10048 = CARTESIAN_POINT('Origin',(-24.25,17.5172318824408,27.2801860892852)) ;
#10049 = CARTESIAN_POINT('',(-24.05,17.2,33.5)) ;
#10050 = CARTESIAN_POINT('',(-24.25,17.2,33.5)) ;
#10051 = CARTESIAN_POINT('Origin',(-24.05,17.5172318824408,27.2801860892852)) ;
#10052 = CARTESIAN_POINT('Origin',(-24.25,17.2261159840305,33.8238840159695)) ;
#10053 = CARTESIAN_POINT('',(-24.05,17.55,33.85)) ;
#10054 = CARTESIAN_POINT('',(-24.25,17.55,33.85)) ;
#10055 = CARTESIAN_POINT('Origin',(-24.05,17.2261159840305,33.8238840159695)) ;
#10056 = CARTESIAN_POINT('Origin',(-24.25,17.55,37.8)) ;
#10057 = CARTESIAN_POINT('',(-24.05,17.55,37.8)) ;
#10058 = CARTESIAN_POINT('',(-24.25,17.55,37.8)) ;
#10059 = CARTESIAN_POINT('',(-24.05,17.55,12.412952685943)) ;
#10060 = CARTESIAN_POINT('Origin',(-24.25,18.75,37.7899579831933)) ;
#10061 = CARTESIAN_POINT('',(-24.05,19.95,37.8)) ;
#10062 = CARTESIAN_POINT('',(-24.25,19.95,37.8)) ;
#10063 = CARTESIAN_POINT('Origin',(-24.05,18.75,37.7899579831933)) ;
#10064 = CARTESIAN_POINT('Origin',(-24.25,19.95,34.)) ;
#10065 = CARTESIAN_POINT('',(-24.05,19.95,34.)) ;
#10066 = CARTESIAN_POINT('',(-24.25,19.95,34.)) ;
#10067 = CARTESIAN_POINT('',(-24.05,19.95,10.512952685943)) ;
#10068 = CARTESIAN_POINT('Origin',(-24.25,21.6437725346931,34.0916800205589)) ;
#10069 = CARTESIAN_POINT('',(-24.05,20.75,32.65)) ;
#10070 = CARTESIAN_POINT('',(-24.25,20.75,32.65)) ;
#10071 = CARTESIAN_POINT('Origin',(-24.05,21.6437725346931,34.0916800205589)) ;
#10072 = CARTESIAN_POINT('Origin',(-24.25,17.453364864871,27.1098816953352)) ;
#10073 = CARTESIAN_POINT('',(-24.05,23.9,27.15)) ;
#10074 = CARTESIAN_POINT('',(-24.25,23.9,27.15)) ;
#10075 = CARTESIAN_POINT('Origin',(-24.05,17.453364864871,27.1098816953352)) ;
#10076 = CARTESIAN_POINT('Origin',(-24.25,23.9,16.95)) ;
#10077 = CARTESIAN_POINT('',(-24.05,23.9,16.95)) ;
#10078 = CARTESIAN_POINT('',(-24.25,23.9,16.95)) ;
#10079 = CARTESIAN_POINT('',(-24.05,23.9,1.98795268594296)) ;
#10080 = CARTESIAN_POINT('Origin',(-24.25,33.4726637867458,16.9651420152427)) ;
#10081 = CARTESIAN_POINT('',(-24.05,26.7,10.2)) ;
#10082 = CARTESIAN_POINT('',(-24.25,26.7,10.2)) ;
#10083 = CARTESIAN_POINT('Origin',(-24.05,33.4726637867458,16.9651420152427)) ;
#10084 = CARTESIAN_POINT('Origin',(-16.3,23.9394766127413,-12.9740946281141)) ;
#10085 = CARTESIAN_POINT('',(-16.3,19.6,36.797821691004)) ;
#10086 = CARTESIAN_POINT('',(-16.3,19.6,37.802178308996)) ;
#10087 = CARTESIAN_POINT('',(-16.3,19.6,12.412952685943)) ;
#10088 = CARTESIAN_POINT('',(-16.3,17.9,36.797821691004)) ;
#10089 = CARTESIAN_POINT('Origin',(-16.3,18.75,36.8151771653543)) ;
#10090 = CARTESIAN_POINT('',(-16.3,17.9,37.8021783089959)) ;
#10091 = CARTESIAN_POINT('',(-16.3,17.9,11.912952685943)) ;
#10092 = CARTESIAN_POINT('Origin',(-16.3,18.75,37.7848228346457)) ;
#10093 = CARTESIAN_POINT('',(-16.3,17.565,31.11)) ;
#10094 = CARTESIAN_POINT('Origin',(-16.3,17.565,27.14)) ;
#10095 = CARTESIAN_POINT('Origin',(-24.05,3.86867726849999,19.973346585625)) ;
#10096 = CARTESIAN_POINT('',(-24.25,3.6,19.9176877660975)) ;
#10097 = CARTESIAN_POINT('',(-24.25,3.86223646644423,19.6990403792266)) ;
#10098 = CARTESIAN_POINT('Origin',(-24.25,3.86867726849999,19.973346585625)) ;
#10099 = CARTESIAN_POINT('Ctrl Pts',(-24.25,3.86223646644423,19.6990403792266)) ;
#10100 = CARTESIAN_POINT('Ctrl Pts',(-24.25,3.86239942575245,19.6980436824252)) ;
#10101 = CARTESIAN_POINT('Ctrl Pts',(-24.2499926106363,3.86256289052268,19.6970470816371)) ;
#10102 = CARTESIAN_POINT('Ctrl Pts',(-24.2495845056741,3.86708910312927,19.6695382704806)) ;
#10103 = CARTESIAN_POINT('Ctrl Pts',(-24.2439612172248,3.87175164288334,19.643414552786)) ;
#10104 = CARTESIAN_POINT('Ctrl Pts',(-24.2230089761414,3.88069316641219,19.595511341096)) ;
#10105 = CARTESIAN_POINT('Ctrl Pts',(-24.2081293684851,3.88489021711545,19.5740942364014)) ;
#10106 = CARTESIAN_POINT('Ctrl Pts',(-24.1710014067334,3.89206056936349,19.5382677000811)) ;
#10107 = CARTESIAN_POINT('Ctrl Pts',(-24.1491881319578,3.89497313876537,19.5241432650165)) ;
#10108 = CARTESIAN_POINT('Ctrl Pts',(-24.1013398303427,3.89895928341784,19.5049329178167)) ;
#10109 = CARTESIAN_POINT('Ctrl Pts',(-24.0757993195191,3.89999999999997,19.5)) ;
#10110 = CARTESIAN_POINT('Ctrl Pts',(-24.05,3.89999999999998,19.5)) ;
#10111 = CARTESIAN_POINT('Ctrl Pts',(-24.25,3.6,19.9176877660975)) ;
#10112 = CARTESIAN_POINT('Ctrl Pts',(-24.25,3.59869799800577,19.9175543222483)) ;
#10113 = CARTESIAN_POINT('Ctrl Pts',(-24.2499872859315,3.59739597782284,19.9174213564527)) ;
#10114 = CARTESIAN_POINT('Ctrl Pts',(-24.2494587398944,3.57033697971399,19.9146677791385)) ;
#10115 = CARTESIAN_POINT('Ctrl Pts',(-24.2439832577742,3.54489668568231,19.9122633488296)) ;
#10116 = CARTESIAN_POINT('Ctrl Pts',(-24.2235688176458,3.49728852286699,19.9079677236395)) ;
#10117 = CARTESIAN_POINT('Ctrl Pts',(-24.2087545540871,3.4756013478467,19.9061195584593)) ;
#10118 = CARTESIAN_POINT('Ctrl Pts',(-24.1716652613261,3.4391536116184,19.90309493138)) ;
#10119 = CARTESIAN_POINT('Ctrl Pts',(-24.1497694510925,3.42472405685893,19.9019445727726)) ;
#10120 = CARTESIAN_POINT('Ctrl Pts',(-24.1016856657977,3.40505796847904,19.9003903114039)) ;
#10121 = CARTESIAN_POINT('Ctrl Pts',(-24.0759688441458,3.4,19.9)) ;
#10122 = CARTESIAN_POINT('Ctrl Pts',(-24.05,3.4,19.9)) ;
#10123 = CARTESIAN_POINT('Origin',(-24.05,7.48858533183141,21.0129348956712)) ;
#10124 = CARTESIAN_POINT('',(-24.25,10.731997720549,22.1880843096407)) ;
#10125 = CARTESIAN_POINT('',(-24.25,7.48858533183141,21.0129348956712)) ;
#10126 = CARTESIAN_POINT('',(-24.05,10.8,22.)) ;
#10127 = CARTESIAN_POINT('Ctrl Pts',(-24.25,10.7319962300761,22.1880837718459)) ;
#10128 = CARTESIAN_POINT('Ctrl Pts',(-24.25,10.7325345967038,22.186594801818)) ;
#10129 = CARTESIAN_POINT('Ctrl Pts',(-24.2499811984774,10.7330729441278,22.1851058839927)) ;
#10130 = CARTESIAN_POINT('Ctrl Pts',(-24.2493432136556,10.7422054198757,22.1598480075178)) ;
#10131 = CARTESIAN_POINT('Ctrl Pts',(-24.2439555708189,10.750683475002,22.136399854346)) ;
#10132 = CARTESIAN_POINT('Ctrl Pts',(-24.2238804494726,10.7667448574682,22.0919777741686)) ;
#10133 = CARTESIAN_POINT('Ctrl Pts',(-24.2091100188948,10.7741400552664,22.0715241613855)) ;
#10134 = CARTESIAN_POINT('Ctrl Pts',(-24.172063647609,10.7865890441546,22.0370925871751)) ;
#10135 = CARTESIAN_POINT('Ctrl Pts',(-24.1501418920773,10.7915238186451,22.0234438094444)) ;
#10136 = CARTESIAN_POINT('Ctrl Pts',(-24.1019690573815,10.7982584799182,22.0048167970724)) ;
#10137 = CARTESIAN_POINT('Ctrl Pts',(-24.0761785376837,10.7999939814428,22.0000166464497)) ;
#10138 = CARTESIAN_POINT('Ctrl Pts',(-24.0500903895948,10.7999999947913,22.0000000144066)) ;
#10139 = CARTESIAN_POINT('Ctrl Pts',(-24.050045194802,10.8,22.)) ;
#10140 = CARTESIAN_POINT('Ctrl Pts',(-24.05,10.8,22.)) ;
#10141 = CARTESIAN_POINT('',(-24.05,7.5567150872414,20.8248967707396)) ;
#10142 = CARTESIAN_POINT('Origin',(-24.05,12.2182755082439,18.0689260404997)) ;
#10143 = CARTESIAN_POINT('',(-24.25,12.9183976933795,22.3916931443706)) ;
#10144 = CARTESIAN_POINT('Origin',(-24.25,12.2182755082439,18.0689260404997)) ;
#10145 = CARTESIAN_POINT('',(-24.05,12.85,22.2)) ;
#10146 = CARTESIAN_POINT('Ctrl Pts',(-24.25,12.9183976933795,22.3916931443706)) ;
#10147 = CARTESIAN_POINT('Ctrl Pts',(-24.25,12.9181668378948,22.3910505718121)) ;
#10148 = CARTESIAN_POINT('Ctrl Pts',(-24.2499966210206,12.9179359974498,22.3904079978316)) ;
#10149 = CARTESIAN_POINT('Ctrl Pts',(-24.2497234095994,12.9086042548365,22.364430144348)) ;
#10150 = CARTESIAN_POINT('Ctrl Pts',(-24.2442064359481,12.8996217972306,22.3393547558271)) ;
#10151 = CARTESIAN_POINT('Ctrl Pts',(-24.223337166426,12.8830080878035,22.2928623998987)) ;
#10152 = CARTESIAN_POINT('Ctrl Pts',(-24.2082563986562,12.8755130699976,22.271828861589)) ;
#10153 = CARTESIAN_POINT('Ctrl Pts',(-24.1706426816821,12.8630621954662,22.2368282591497)) ;
#10154 = CARTESIAN_POINT('Ctrl Pts',(-24.1486086719302,12.858181652241,22.2230759619812)) ;
#10155 = CARTESIAN_POINT('Ctrl Pts',(-24.1007404646662,12.8516575377895,22.2046806927339)) ;
#10156 = CARTESIAN_POINT('Ctrl Pts',(-24.0755026160457,12.85,22.2)) ;
#10157 = CARTESIAN_POINT('Ctrl Pts',(-24.05,12.85,22.2)) ;
#10158 = CARTESIAN_POINT('Origin',(-24.05,12.2182755082439,18.0689260404997)) ;
#10159 = CARTESIAN_POINT('Origin',(-24.05,24.7469152941988,15.4731262457782)) ;
#10160 = CARTESIAN_POINT('',(-24.25,15.63399980594,20.8033220974013)) ;
#10161 = CARTESIAN_POINT('',(-24.25,24.7469152941988,15.4731262457782)) ;
#10162 = CARTESIAN_POINT('',(-24.05,15.5,20.65)) ;
#10163 = CARTESIAN_POINT('Ctrl Pts',(-24.25,15.63399980594,20.8033220974013)) ;
#10164 = CARTESIAN_POINT('Ctrl Pts',(-24.25,15.6335509952832,20.8028060276234)) ;
#10165 = CARTESIAN_POINT('Ctrl Pts',(-24.2499966124945,15.6331021746881,20.8022899714547)) ;
#10166 = CARTESIAN_POINT('Ctrl Pts',(-24.249722940117,15.614972088751,20.7814449197118)) ;
#10167 = CARTESIAN_POINT('Ctrl Pts',(-24.2442012683717,15.5974573764528,20.7613477431599)) ;
#10168 = CARTESIAN_POINT('Ctrl Pts',(-24.2233158935857,15.5649632480559,20.7241280374561)) ;
#10169 = CARTESIAN_POINT('Ctrl Pts',(-24.2082248717087,15.5502511678181,20.7073104617596)) ;
#10170 = CARTESIAN_POINT('Ctrl Pts',(-24.1705925293635,15.5257656936601,20.6793548187585)) ;
#10171 = CARTESIAN_POINT('Ctrl Pts',(-24.1485538369899,15.5161408054958,20.6683845338974)) ;
#10172 = CARTESIAN_POINT('Ctrl Pts',(-24.1006977684759,15.5032739399685,20.653725811144)) ;
#10173 = CARTESIAN_POINT('Ctrl Pts',(-24.0754813864138,15.5,20.65)) ;
#10174 = CARTESIAN_POINT('Ctrl Pts',(-24.05,15.5,20.65)) ;
#10175 = CARTESIAN_POINT('',(-24.05,24.6459386311912,15.3004887251523)) ;
#10176 = CARTESIAN_POINT('Origin',(-24.05,12.5256959686759,18.3486581187154)) ;
#10177 = CARTESIAN_POINT('',(-24.25,16.39481890426,19.1953078115317)) ;
#10178 = CARTESIAN_POINT('Origin',(-24.25,12.5256959686759,18.3486581187154)) ;
#10179 = CARTESIAN_POINT('',(-24.05,16.2,19.15)) ;
#10180 = CARTESIAN_POINT('Ctrl Pts',(-24.25,16.39481890426,19.1953078115317)) ;
#10181 = CARTESIAN_POINT('Ctrl Pts',(-24.25,16.3937985287439,19.195070324616)) ;
#10182 = CARTESIAN_POINT('Ctrl Pts',(-24.2499917696977,16.3927781683397,19.1948328440442)) ;
#10183 = CARTESIAN_POINT('Ctrl Pts',(-24.2495687833023,16.3665596763747,19.1887307763402)) ;
#10184 = CARTESIAN_POINT('Ctrl Pts',(-24.2441462640923,16.3416754708443,19.1829410368979)) ;
#10185 = CARTESIAN_POINT('Ctrl Pts',(-24.2238050373329,16.2951486910567,19.1721187037123)) ;
#10186 = CARTESIAN_POINT('Ctrl Pts',(-24.2090186613912,16.2739730545514,19.1671947135444)) ;
#10187 = CARTESIAN_POINT('Ctrl Pts',(-24.1719464410901,16.2383357459206,19.1589095136144)) ;
#10188 = CARTESIAN_POINT('Ctrl Pts',(-24.150015697699,16.2242141206252,19.1556273129937)) ;
#10189 = CARTESIAN_POINT('Ctrl Pts',(-24.1018323209062,16.2049543635143,19.1511512193477)) ;
#10190 = CARTESIAN_POINT('Ctrl Pts',(-24.0760407121131,16.2,19.15)) ;
#10191 = CARTESIAN_POINT('Ctrl Pts',(-24.05,16.2,19.15)) ;
#10192 = CARTESIAN_POINT('Origin',(-24.05,12.5256959686759,18.3486581187154)) ;
#10193 = CARTESIAN_POINT('Origin',(-24.05,17.75,12.412952685943)) ;
#10194 = CARTESIAN_POINT('',(-24.25,17.75,37.799163194566)) ;
#10195 = CARTESIAN_POINT('Ctrl Pts',(-24.05,17.55,37.8)) ;
#10196 = CARTESIAN_POINT('Ctrl Pts',(-24.0632701694844,17.55,37.7999646531197)) ;
#10197 = CARTESIAN_POINT('Ctrl Pts',(-24.0765399924102,17.5513250740506,37.7999293062395)) ;
#10198 = CARTESIAN_POINT('Ctrl Pts',(-24.0895481340208,17.5539491262568,37.7998939593592)) ;
#10199 = CARTESIAN_POINT('Ctrl Pts',(-24.1025532968563,17.5565725775731,37.7998586205732)) ;
#10200 = CARTESIAN_POINT('Ctrl Pts',(-24.1152962197139,17.5604942733101,37.7998232817871)) ;
#10201 = CARTESIAN_POINT('Ctrl Pts',(-24.1275260588055,17.5656370150868,37.799787943001)) ;
#10202 = CARTESIAN_POINT('Ctrl Pts',(-24.1397534773073,17.5707787389869,37.7997526112094)) ;
#10203 = CARTESIAN_POINT('Ctrl Pts',(-24.1514673780366,17.5771407558669,37.7997172794177)) ;
#10204 = CARTESIAN_POINT('Ctrl Pts',(-24.1624372641837,17.5845978790254,37.7996819476261)) ;
#10205 = CARTESIAN_POINT('Ctrl Pts',(-24.1734053194263,17.5920537575693,37.7996466217314)) ;
#10206 = CARTESIAN_POINT('Ctrl Pts',(-24.1836290375724,17.6006039870742,37.7996112958368)) ;
#10207 = CARTESIAN_POINT('Ctrl Pts',(-24.1929073111899,17.6100803787581,37.7995759699421)) ;
#10208 = CARTESIAN_POINT('Ctrl Pts',(-24.2021908572985,17.6195621555162,37.7995406239731)) ;
#10209 = CARTESIAN_POINT('Ctrl Pts',(-24.2105273961139,17.6299706560222,37.7995052780041)) ;
#10210 = CARTESIAN_POINT('Ctrl Pts',(-24.2177527569689,17.6411009066643,37.799469932035)) ;
#10211 = CARTESIAN_POINT('Ctrl Pts',(-24.2249750808544,17.6522264790305,37.7994346009226)) ;
#10212 = CARTESIAN_POINT('Ctrl Pts',(-24.2310867869367,17.6640726125166,37.7993992698103)) ;
#10213 = CARTESIAN_POINT('Ctrl Pts',(-24.2359676185276,17.6764062172518,37.7993639386979)) ;
#10214 = CARTESIAN_POINT('Ctrl Pts',(-24.2408502551657,17.6887443832466,37.7993285945192)) ;
#10215 = CARTESIAN_POINT('Ctrl Pts',(-24.2445008489509,17.7015697384064,37.7992932503405)) ;
#10216 = CARTESIAN_POINT('Ctrl Pts',(-24.2468475163264,17.7146297396653,37.7992579061619)) ;
#10217 = CARTESIAN_POINT('Ctrl Pts',(-24.2489436334282,17.7262953435236,37.7992263356299)) ;
#10218 = CARTESIAN_POINT('Ctrl Pts',(-24.25,17.7381475732323,37.799194765098)) ;
#10219 = CARTESIAN_POINT('Ctrl Pts',(-24.25,17.75,37.799163194566)) ;
#10220 = CARTESIAN_POINT('',(-24.25,17.75,33.8570883563437)) ;
#10221 = CARTESIAN_POINT('',(-24.25,17.75,12.412952685943)) ;
#10222 = CARTESIAN_POINT('Ctrl Pts',(-24.25,17.75,33.8570883563437)) ;
#10223 = CARTESIAN_POINT('Ctrl Pts',(-24.25,17.7483048927981,33.8570346913132)) ;
#10224 = CARTESIAN_POINT('Ctrl Pts',(-24.2499784495869,17.7466098579761,33.8569808984569)) ;
#10225 = CARTESIAN_POINT('Ctrl Pts',(-24.2492934706748,17.7196757862012,33.8561240343194)) ;
#10226 = CARTESIAN_POINT('Ctrl Pts',(-24.2438780635363,17.6947845328972,33.8553018126003)) ;
#10227 = CARTESIAN_POINT('Ctrl Pts',(-24.2237614818921,17.6476026569698,33.8536820465369)) ;
#10228 = CARTESIAN_POINT('Ctrl Pts',(-24.2089645660017,17.6258680589014,33.8529014445044)) ;
#10229 = CARTESIAN_POINT('Ctrl Pts',(-24.1718827931726,17.5893078527847,33.8515452810162)) ;
#10230 = CARTESIAN_POINT('Ctrl Pts',(-24.1499574522595,17.5748252688856,33.8509836241205)) ;
#10231 = CARTESIAN_POINT('Ctrl Pts',(-24.1017958701297,17.555078893135,33.8502065060916)) ;
#10232 = CARTESIAN_POINT('Ctrl Pts',(-24.0760230373047,17.55,33.85)) ;
#10233 = CARTESIAN_POINT('Ctrl Pts',(-24.05,17.55,33.85)) ;
#10234 = CARTESIAN_POINT('Origin',(-24.05,29.7633733578399,-15.291248496029)) ;
#10235 = CARTESIAN_POINT('',(-24.05,35.4,-9.7)) ;
#10236 = CARTESIAN_POINT('',(-24.25,35.541707130624,-9.55886443234855)) ;
#10237 = CARTESIAN_POINT('Ctrl Pts',(-24.05,35.4,-9.7)) ;
#10238 = CARTESIAN_POINT('Ctrl Pts',(-24.0632701694643,35.3999882729118,-9.69998817773565)) ;
#10239 = CARTESIAN_POINT('Ctrl Pts',(-24.0765399923701,35.4009172937257,-9.6990431810638)) ;
#10240 = CARTESIAN_POINT('Ctrl Pts',(-24.0895481339619,35.4027685180476,-9.69718337031635)) ;
#10241 = CARTESIAN_POINT('Ctrl Pts',(-24.1025532967779,35.4046193184517,-9.6953239854529)) ;
#10242 = CARTESIAN_POINT('Ctrl Pts',(-24.1152962196173,35.4073918013753,-9.69255030317433)) ;
#10243 = CARTESIAN_POINT('Ctrl Pts',(-24.1275260586929,35.4110311429201,-9.68891667355651)) ;
#10244 = CARTESIAN_POINT('Ctrl Pts',(-24.139753477178,35.4146697641483,-9.68528376312474)) ;
#10245 = CARTESIAN_POINT('Ctrl Pts',(-24.1514673778929,35.4191747093011,-9.68079143563539)) ;
#10246 = CARTESIAN_POINT('Ctrl Pts',(-24.1624372640292,35.4244570869814,-9.67552783886286)) ;
#10247 = CARTESIAN_POINT('Ctrl Pts',(-24.1734053192599,35.4297385830177,-9.67026512059973)) ;
#10248 = CARTESIAN_POINT('Ctrl Pts',(-24.1836290373979,35.4357969752947,-9.66423166493807)) ;
#10249 = CARTESIAN_POINT('Ctrl Pts',(-24.1929073110115,35.4425128458928,-9.65754590678402)) ;
#10250 = CARTESIAN_POINT('Ctrl Pts',(-24.2021908571152,35.4492325328647,-9.65085634936783)) ;
#10251 = CARTESIAN_POINT('Ctrl Pts',(-24.2105273959302,35.4566100967359,-9.64351409386539)) ;
#10252 = CARTESIAN_POINT('Ctrl Pts',(-24.2177527567903,35.4645000078171,-9.63566348462498)) ;
#10253 = CARTESIAN_POINT('Ctrl Pts',(-24.2249750806803,35.4723866026039,-9.62781617515956)) ;
#10254 = CARTESIAN_POINT('Ctrl Pts',(-24.2310867867725,35.4807847004745,-9.61946134933943)) ;
#10255 = CARTESIAN_POINT('Ctrl Pts',(-24.235967618379,35.4895288148778,-9.61076315675825)) ;
#10256 = CARTESIAN_POINT('Ctrl Pts',(-24.2408502550324,35.4982761630614,-9.6020617473797)) ;
#10257 = CARTESIAN_POINT('Ctrl Pts',(-24.2445008488388,35.5073693274479,-9.5930171698336)) ;
#10258 = CARTESIAN_POINT('Ctrl Pts',(-24.2468475162411,35.5166290153408,-9.58380727835446)) ;
#10259 = CARTESIAN_POINT('Ctrl Pts',(-24.2489436333995,35.52490005991,-9.57558071350875)) ;
#10260 = CARTESIAN_POINT('Ctrl Pts',(-24.25,35.5333035489127,-9.56722266607385)) ;
#10261 = CARTESIAN_POINT('Ctrl Pts',(-24.25,35.541707130624,-9.55886443234855)) ;
#10262 = CARTESIAN_POINT('',(-24.25,37.8999308547965,-15.5052586405422)) ;
#10263 = CARTESIAN_POINT('Origin',(-24.25,29.7633733578399,-15.291248496029)) ;
#10264 = CARTESIAN_POINT('',(-24.05,37.7,-15.5)) ;
#10265 = CARTESIAN_POINT('Origin',(-24.05,37.8999308547965,-15.5052586405422)) ;
#10266 = CARTESIAN_POINT('Origin',(-24.05,29.7633733578399,-15.291248496029)) ;
#10267 = CARTESIAN_POINT('Origin',(-24.05,37.9279179147939,-14.4204278690655)) ;
#10268 = CARTESIAN_POINT('',(-24.05,36.65,-56.2)) ;
#10269 = CARTESIAN_POINT('',(-24.05,37.7279844379825,-14.415269880106)) ;
#10270 = CARTESIAN_POINT('',(-24.25,36.8459456848986,-56.3597323992937)) ;
#10271 = CARTESIAN_POINT('',(-24.25,37.9279179147939,-14.4204278690655)) ;
#10272 = CARTESIAN_POINT('Ctrl Pts',(-24.25,36.8459456848986,-56.3597323992937)) ;
#10273 = CARTESIAN_POINT('Ctrl Pts',(-24.25,36.8452932432196,-56.3591906677191)) ;
#10274 = CARTESIAN_POINT('Ctrl Pts',(-24.2499966713728,36.8446407490717,-56.3586489949844)) ;
#10275 = CARTESIAN_POINT('Ctrl Pts',(-24.2498073839985,36.826091678425,-56.3432532583288)) ;
#10276 = CARTESIAN_POINT('Ctrl Pts',(-24.2471193144542,36.8081301664191,-56.3284236042304)) ;
#10277 = CARTESIAN_POINT('Ctrl Pts',(-24.2367641356701,36.7736693811156,-56.3001110660321)) ;
#10278 = CARTESIAN_POINT('Ctrl Pts',(-24.2292318720098,36.7570768798035,-56.2865472202178)) ;
#10279 = CARTESIAN_POINT('Ctrl Pts',(-24.2064522017498,36.7216811428078,-56.2577328860845)) ;
#10280 = CARTESIAN_POINT('Ctrl Pts',(-24.1896672437335,36.7034378018957,-56.2429732328781)) ;
#10281 = CARTESIAN_POINT('Ctrl Pts',(-24.1519096063163,36.6760935350204,-56.220928962173)) ;
#10282 = CARTESIAN_POINT('Ctrl Pts',(-24.132484884718,36.6660883821569,-56.2128959810192)) ;
#10283 = CARTESIAN_POINT('Ctrl Pts',(-24.0915642364822,36.653234532305,-56.2025876834372)) ;
#10284 = CARTESIAN_POINT('Ctrl Pts',(-24.0709835762204,36.65,-56.2)) ;
#10285 = CARTESIAN_POINT('Ctrl Pts',(-24.05,36.65,-56.2)) ;
#10286 = CARTESIAN_POINT('Origin',(-24.05,18.75,37.7899579831933)) ;
#10287 = CARTESIAN_POINT('',(-24.25,19.7499996500575,37.7991631591148)) ;
#10288 = CARTESIAN_POINT('Ctrl Pts',(-24.05,19.95,37.8)) ;
#10289 = CARTESIAN_POINT('Ctrl Pts',(-24.0632701637967,19.9499996450624,37.8000424142976)) ;
#10290 = CARTESIAN_POINT('Ctrl Pts',(-24.0765399810356,19.94867426136,37.8000737393719)) ;
#10291 = CARTESIAN_POINT('Ctrl Pts',(-24.0895481172947,19.9460499473545,37.8000937776279)) ;
#10292 = CARTESIAN_POINT('Ctrl Pts',(-24.1025532746016,19.9434262343348,37.8001138112951)) ;
#10293 = CARTESIAN_POINT('Ctrl Pts',(-24.1152961922746,19.9395043247711,37.8001225626839)) ;
#10294 = CARTESIAN_POINT('Ctrl Pts',(-24.1275260268481,19.9343614175846,37.8001202894756)) ;
#10295 = CARTESIAN_POINT('Ctrl Pts',(-24.1397534405889,19.92921952841,37.8001180167172)) ;
#10296 = CARTESIAN_POINT('Ctrl Pts',(-24.1514673372456,19.9228573947066,37.8001047243444)) ;
#10297 = CARTESIAN_POINT('Ctrl Pts',(-24.1624372203003,19.915400201571,37.8000811250022)) ;
#10298 = CARTESIAN_POINT('Ctrl Pts',(-24.1734052721897,19.9079442532392,37.8000575295993)) ;
#10299 = CARTESIAN_POINT('Ctrl Pts',(-24.1836289879996,19.899394000828,37.8000236325339)) ;
#10300 = CARTESIAN_POINT('Ctrl Pts',(-24.1929072605376,19.8899176293381,37.7999805824503)) ;
#10301 = CARTESIAN_POINT('Ctrl Pts',(-24.2021908052356,19.8804358731232,37.7999375079045)) ;
#10302 = CARTESIAN_POINT('Ctrl Pts',(-24.2105273439674,19.8700274363687,37.7998852729588)) ;
#10303 = CARTESIAN_POINT('Ctrl Pts',(-24.2177527062381,19.8588972867723,37.7998254284371)) ;
#10304 = CARTESIAN_POINT('Ctrl Pts',(-24.2249750314017,19.8477718156204,37.7997656090704)) ;
#10305 = CARTESIAN_POINT('Ctrl Pts',(-24.231086740303,19.8359258206247,37.7996981907095)) ;
#10306 = CARTESIAN_POINT('Ctrl Pts',(-24.2359675763273,19.8235923837952,37.7996250677075)) ;
#10307 = CARTESIAN_POINT('Ctrl Pts',(-24.2408502173167,19.8112543859802,37.7995519176641)) ;
#10308 = CARTESIAN_POINT('Ctrl Pts',(-24.2445008171118,19.7984292284339,37.7994730638621)) ;
#10309 = CARTESIAN_POINT('Ctrl Pts',(-24.2468474921171,19.7853694446507,37.7993906788029)) ;
#10310 = CARTESIAN_POINT('Ctrl Pts',(-24.2489436252733,19.7737039836308,37.7993170895528)) ;
#10311 = CARTESIAN_POINT('Ctrl Pts',(-24.25,19.7618519109258,37.7992406894262)) ;
#10312 = CARTESIAN_POINT('Ctrl Pts',(-24.25,19.7499996500575,37.7991631591148)) ;
#10313 = CARTESIAN_POINT('Origin',(-24.25,18.75,37.7899579831933)) ;
#10314 = CARTESIAN_POINT('Origin',(-24.05,37.7318176617063,-60.502128268216)) ;
#10315 = CARTESIAN_POINT('',(-24.25,41.9506268879595,-60.8840463309467)) ;
#10316 = CARTESIAN_POINT('Origin',(-24.25,37.7318176617063,-60.502128268216)) ;
#10317 = CARTESIAN_POINT('',(-24.05,42.15,-60.9)) ;
#10318 = CARTESIAN_POINT('Ctrl Pts',(-24.25,41.9506268879594,-60.8840463309467)) ;
#10319 = CARTESIAN_POINT('Ctrl Pts',(-24.25,41.9517471911499,-60.8841361107773)) ;
#10320 = CARTESIAN_POINT('Ctrl Pts',(-24.2499905274602,41.9528674746358,-60.884225886703)) ;
#10321 = CARTESIAN_POINT('Ctrl Pts',(-24.2495367852489,41.9796968068967,-60.8863758483662)) ;
#10322 = CARTESIAN_POINT('Ctrl Pts',(-24.2441168334782,42.0050812395976,-60.8884087660416)) ;
#10323 = CARTESIAN_POINT('Ctrl Pts',(-24.2238077082346,42.0526243758534,-60.8922143172946)) ;
#10324 = CARTESIAN_POINT('Ctrl Pts',(-24.2090218955104,42.074295218724,-60.893947902738)) ;
#10325 = CARTESIAN_POINT('Ctrl Pts',(-24.1719501690967,42.1107665799089,-60.8968644715332)) ;
#10326 = CARTESIAN_POINT('Ctrl Pts',(-24.1500190632069,42.1252187814051,-60.8980196294303)) ;
#10327 = CARTESIAN_POINT('Ctrl Pts',(-24.1018344050974,42.1449296139692,-60.8995949062453)) ;
#10328 = CARTESIAN_POINT('Ctrl Pts',(-24.0760417263098,42.15,-60.8999999999999)) ;
#10329 = CARTESIAN_POINT('Ctrl Pts',(-24.05,42.1500000000001,-60.8999999999991)) ;
#10330 = CARTESIAN_POINT('Origin',(-24.05,37.7318176617063,-60.502128268216)) ;
#10331 = CARTESIAN_POINT('Origin',(-24.05,43.5701155187154,-37.6713759567788)) ;
#10332 = CARTESIAN_POINT('',(-24.25,42.1003608664925,-58.7378593416195)) ;
#10333 = CARTESIAN_POINT('',(-24.25,43.5701155187154,-37.6713759567788)) ;
#10334 = CARTESIAN_POINT('',(-24.05,42.3,-58.75)) ;
#10335 = CARTESIAN_POINT('Origin',(-24.05,42.1003608738345,-58.7378592000713)) ;
#10336 = CARTESIAN_POINT('',(-24.05,43.7696305388826,-37.6852956093486)) ;
#10337 = CARTESIAN_POINT('Origin',(-24.05,33.4726637867458,16.9651420152427)) ;
#10338 = CARTESIAN_POINT('',(-24.25,23.7000000012803,16.9498418202582)) ;
#10339 = CARTESIAN_POINT('Ctrl Pts',(-24.25,23.7000000012803,16.9498418202582)) ;
#10340 = CARTESIAN_POINT('Ctrl Pts',(-24.25,23.7132701649591,16.9498559146256)) ;
#10341 = CARTESIAN_POINT('Ctrl Pts',(-24.24867492595,23.7265399820437,16.9498700358474)) ;
#10342 = CARTESIAN_POINT('Ctrl Pts',(-24.2460508737449,23.7395481180995,16.9498837737012)) ;
#10343 = CARTESIAN_POINT('Ctrl Pts',(-24.2434274224297,23.7525532753816,16.9498975084091)) ;
#10344 = CARTESIAN_POINT('Ctrl Pts',(-24.2395057266942,23.765296192973,16.9499108588538)) ;
#10345 = CARTESIAN_POINT('Ctrl Pts',(-24.2343629849196,23.7775260273978,16.9499234291553)) ;
#10346 = CARTESIAN_POINT('Ctrl Pts',(-24.2292212610216,23.7897534412339,16.9499359969688)) ;
#10347 = CARTESIAN_POINT('Ctrl Pts',(-24.222859244144,23.8014673378977,16.949947783934)) ;
#10348 = CARTESIAN_POINT('Ctrl Pts',(-24.2154021209883,23.8124372208699,16.9499584241338)) ;
#10349 = CARTESIAN_POINT('Ctrl Pts',(-24.2079462424471,23.8234052729382,16.9499690625578)) ;
#10350 = CARTESIAN_POINT('Ctrl Pts',(-24.1993960129453,23.8336289888011,16.9499785536818)) ;
#10351 = CARTESIAN_POINT('Ctrl Pts',(-24.1899196212647,23.8429072612832,16.9499865760112)) ;
#10352 = CARTESIAN_POINT('Ctrl Pts',(-24.1804378445097,23.8521908062561,16.9499946028994)) ;
#10353 = CARTESIAN_POINT('Ctrl Pts',(-24.1700293440071,23.8605273450856,16.9500011585298)) ;
#10354 = CARTESIAN_POINT('Ctrl Pts',(-24.1588990933682,23.8677527073182,16.9500059780284)) ;
#10355 = CARTESIAN_POINT('Ctrl Pts',(-24.1477735210053,23.8749750325807,16.9500107955012)) ;
#10356 = CARTESIAN_POINT('Ctrl Pts',(-24.1359273875225,23.8810867414029,16.9500138776823)) ;
#10357 = CARTESIAN_POINT('Ctrl Pts',(-24.1235937827905,23.8859675772572,16.9500150277399)) ;
#10358 = CARTESIAN_POINT('Ctrl Pts',(-24.1112556167988,23.8908502181604,16.9500161782227)) ;
#10359 = CARTESIAN_POINT('Ctrl Pts',(-24.0984302616419,23.8945008177358,16.9500153947128)) ;
#10360 = CARTESIAN_POINT('Ctrl Pts',(-24.0853702603857,23.8968474925285,16.9500125559086)) ;
#10361 = CARTESIAN_POINT('Ctrl Pts',(-24.0737046565109,23.898943616259,16.9500100201995)) ;
#10362 = CARTESIAN_POINT('Ctrl Pts',(-24.061852426785,23.8999999907535,16.9500058455726)) ;
#10363 = CARTESIAN_POINT('Ctrl Pts',(-24.05,23.9,16.95)) ;
#10364 = CARTESIAN_POINT('',(-24.25,26.5585000901577,10.0586572410252)) ;
#10365 = CARTESIAN_POINT('Origin',(-24.05,26.5585000901577,10.0586572410252)) ;
#10366 = CARTESIAN_POINT('Origin',(-24.25,33.4726637867458,16.9651420152427)) ;
#10367 = CARTESIAN_POINT('Origin',(-24.05,37.4869714539765,-0.869814166451149)) ;
#10368 = CARTESIAN_POINT('',(-24.05,38.35,-1.45)) ;
#10369 = CARTESIAN_POINT('',(-24.25,38.2088062765873,-1.59164898906192)) ;
#10370 = CARTESIAN_POINT('Ctrl Pts',(-24.05,38.35,-1.45)) ;
#10371 = CARTESIAN_POINT('Ctrl Pts',(-24.0632701694844,38.35000961527,-1.45000961527001)) ;
#10372 = CARTESIAN_POINT('Ctrl Pts',(-24.0765399924102,38.3490822616933,-1.45095619938675)) ;
#10373 = CARTESIAN_POINT('Ctrl Pts',(-24.0895481340208,38.3472363918541,-1.45282129976597)) ;
#10374 = CARTESIAN_POINT('Ctrl Pts',(-24.1025532968563,38.3453909447064,-1.45468597305001)) ;
#10375 = CARTESIAN_POINT('Ctrl Pts',(-24.1152962197139,38.3426275001252,-1.4574686437676)) ;
#10376 = CARTESIAN_POINT('Ctrl Pts',(-24.1275260588055,38.3390006456092,-1.46111472441998)) ;
#10377 = CARTESIAN_POINT('Ctrl Pts',(-24.1397534773073,38.335374508938,-1.4647600834222)) ;
#10378 = CARTESIAN_POINT('Ctrl Pts',(-24.1514673780366,38.3308854948256,-1.46926831986561)) ;
#10379 = CARTESIAN_POINT('Ctrl Pts',(-24.1624372641837,38.3256221236376,-1.47455091338466)) ;
#10380 = CARTESIAN_POINT('Ctrl Pts',(-24.1734053194263,38.3203596309209,-1.47983262522414)) ;
#10381 = CARTESIAN_POINT('Ctrl Pts',(-24.1836290375724,38.3143233152186,-1.48588816004911)) ;
#10382 = CARTESIAN_POINT('Ctrl Pts',(-24.1929073111898,38.3076321039592,-1.49259859043134)) ;
#10383 = CARTESIAN_POINT('Ctrl Pts',(-24.2021908572985,38.3009370903379,-1.49931283409685)) ;
#10384 = CARTESIAN_POINT('Ctrl Pts',(-24.2105273961138,38.2935867840703,-1.50668237040873)) ;
#10385 = CARTESIAN_POINT('Ctrl Pts',(-24.2177527569689,38.2857261233871,-1.51456226113624)) ;
#10386 = CARTESIAN_POINT('Ctrl Pts',(-24.2249750808544,38.2778687667031,-1.52243883978168)) ;
#10387 = CARTESIAN_POINT('Ctrl Pts',(-24.2310867869367,38.269501896365,-1.53082493208131)) ;
#10388 = CARTESIAN_POINT('Ctrl Pts',(-24.2359676185276,38.260790331801,-1.53955571860678)) ;
#10389 = CARTESIAN_POINT('Ctrl Pts',(-24.2408502551657,38.2520755454938,-1.54828973398417)) ;
#10390 = CARTESIAN_POINT('Ctrl Pts',(-24.2445008489509,38.2430162644243,-1.55736824412392)) ;
#10391 = CARTESIAN_POINT('Ctrl Pts',(-24.2468475163264,38.2337910635069,-1.5666126741115)) ;
#10392 = CARTESIAN_POINT('Ctrl Pts',(-24.2489436334282,38.2255508239172,-1.5748700897115)) ;
#10393 = CARTESIAN_POINT('Ctrl Pts',(-24.25,38.2171786199231,-1.58325946971581)) ;
#10394 = CARTESIAN_POINT('Ctrl Pts',(-24.25,38.2088062765873,-1.59164898906192)) ;
#10395 = CARTESIAN_POINT('',(-24.25,37.4869714539765,-0.869814166451149)) ;
#10396 = CARTESIAN_POINT('',(-24.05,37.6283928102138,-0.72839281021384)) ;
#10397 = CARTESIAN_POINT('Origin',(-24.05,23.7,1.98795268594296)) ;
#10398 = CARTESIAN_POINT('',(-24.25,23.6999999690425,27.1493776857403)) ;
#10399 = CARTESIAN_POINT('',(-24.25,23.7,1.98795268594296)) ;
#10400 = CARTESIAN_POINT('Ctrl Pts',(-24.25,23.7000000155168,27.1493727892866)) ;
#10401 = CARTESIAN_POINT('Ctrl Pts',(-24.2499999998777,23.7015760333225,27.1493777710123)) ;
#10402 = CARTESIAN_POINT('Ctrl Pts',(-24.2499813712591,23.703151980566,27.1493827515679)) ;
#10403 = CARTESIAN_POINT('Ctrl Pts',(-24.2493452398792,23.7300560876817,27.1494677621689)) ;
#10404 = CARTESIAN_POINT('Ctrl Pts',(-24.2439389270727,23.7550416809086,27.1495464596794)) ;
#10405 = CARTESIAN_POINT('Ctrl Pts',(-24.2238108181396,23.802313411751,27.1496949552354)) ;
#10406 = CARTESIAN_POINT('Ctrl Pts',(-24.2090255878345,23.824052809064,27.1497630282056)) ;
#10407 = CARTESIAN_POINT('Ctrl Pts',(-24.1719543545186,23.8606404855449,27.1498773846942)) ;
#10408 = CARTESIAN_POINT('Ctrl Pts',(-24.15002280892,23.8751390022258,27.1499225811516)) ;
#10409 = CARTESIAN_POINT('Ctrl Pts',(-24.1018367027478,23.8949132761296,27.1499841811619)) ;
#10410 = CARTESIAN_POINT('Ctrl Pts',(-24.0760428468437,23.9,27.1499999999993)) ;
#10411 = CARTESIAN_POINT('Ctrl Pts',(-24.05,23.9,27.1499999999993)) ;
#10412 = CARTESIAN_POINT('Origin',(-24.05,23.7122919887408,-16.1822567109578)) ;
#10413 = CARTESIAN_POINT('',(-24.05,44.45,-17.3)) ;
#10414 = CARTESIAN_POINT('',(-24.25,44.2502789868947,-17.2894378848858)) ;
#10415 = CARTESIAN_POINT('Ctrl Pts',(-24.05,44.45,-17.3)) ;
#10416 = CARTESIAN_POINT('Ctrl Pts',(-24.0632701694836,44.4499995354581,-17.3000086187351)) ;
#10417 = CARTESIAN_POINT('Ctrl Pts',(-24.0765399924086,44.4486759174207,-17.2999459207093)) ;
#10418 = CARTESIAN_POINT('Ctrl Pts',(-24.0895481340185,44.4460552042224,-17.2998133055442)) ;
#10419 = CARTESIAN_POINT('Ctrl Pts',(-24.1025532968532,44.4434350911495,-17.299680720747)) ;
#10420 = CARTESIAN_POINT('Ctrl Pts',(-24.1152962197101,44.4395186155883,-17.2994782582822)) ;
#10421 = CARTESIAN_POINT('Ctrl Pts',(-24.127526058801,44.4343828642744,-17.2992100684806)) ;
#10422 = CARTESIAN_POINT('Ctrl Pts',(-24.1397534773022,44.4292481294536,-17.2989419317604)) ;
#10423 = CARTESIAN_POINT('Ctrl Pts',(-24.1514673780309,44.4228948708492,-17.2986081082184)) ;
#10424 = CARTESIAN_POINT('Ctrl Pts',(-24.1624372641776,44.4154480939293,-17.2982153315896)) ;
#10425 = CARTESIAN_POINT('Ctrl Pts',(-24.1734053194197,44.4080025598972,-17.2978226205164)) ;
#10426 = CARTESIAN_POINT('Ctrl Pts',(-24.1836290375656,44.399464261773,-17.2973709969963)) ;
#10427 = CARTESIAN_POINT('Ctrl Pts',(-24.1929073111829,44.39000114473,-17.2968695100719)) ;
#10428 = CARTESIAN_POINT('Ctrl Pts',(-24.2021908572913,44.3805326501562,-17.2963677381714)) ;
#10429 = CARTESIAN_POINT('Ctrl Pts',(-24.2105273961066,44.3701387759104,-17.2958160726108)) ;
#10430 = CARTESIAN_POINT('Ctrl Pts',(-24.2177527569619,44.3590241986199,-17.2952255433351)) ;
#10431 = CARTESIAN_POINT('Ctrl Pts',(-24.2249750808476,44.3479142930177,-17.2946352622711)) ;
#10432 = CARTESIAN_POINT('Ctrl Pts',(-24.2310867869303,44.3360848716631,-17.2940061814933)) ;
#10433 = CARTESIAN_POINT('Ctrl Pts',(-24.2359676185217,44.3237686866229,-17.2933508454617)) ;
#10434 = CARTESIAN_POINT('Ctrl Pts',(-24.2408502551605,44.3114479467653,-17.2926952670713)) ;
#10435 = CARTESIAN_POINT('Ctrl Pts',(-24.2445008489465,44.298640724898,-17.2920134485918)) ;
#10436 = CARTESIAN_POINT('Ctrl Pts',(-24.246847516323,44.2855991980142,-17.2913189828271)) ;
#10437 = CARTESIAN_POINT('Ctrl Pts',(-24.2489436334271,44.2739500960415,-17.2906986641649)) ;
#10438 = CARTESIAN_POINT('Ctrl Pts',(-24.25,44.2621146394998,-17.2900682864539)) ;
#10439 = CARTESIAN_POINT('Ctrl Pts',(-24.25,44.2502789868947,-17.2894378848858)) ;
#10440 = CARTESIAN_POINT('Origin',(-24.25,23.7122919887408,-16.1822567109578)) ;
#10441 = CARTESIAN_POINT('Origin',(-24.05,23.7122919887408,-16.1822567109578)) ;
#10442 = CARTESIAN_POINT('Origin',(-24.05,17.453364864871,27.1098816953352)) ;
#10443 = CARTESIAN_POINT('',(-24.25,20.6462198057264,32.4790238413936)) ;
#10444 = CARTESIAN_POINT('Origin',(-24.25,17.453364864871,27.1098816953352)) ;
#10445 = CARTESIAN_POINT('Ctrl Pts',(-24.25,20.6462198057264,32.4790238413936)) ;
#10446 = CARTESIAN_POINT('Ctrl Pts',(-24.25,20.6467552570576,32.4799066099211)) ;
#10447 = CARTESIAN_POINT('Ctrl Pts',(-24.2499920056975,20.6472907045759,32.4807893626782)) ;
#10448 = CARTESIAN_POINT('Ctrl Pts',(-24.2495751592316,20.6612498771786,32.5038025845034)) ;
#10449 = CARTESIAN_POINT('Ctrl Pts',(-24.2441531700626,20.6745092215521,32.5256560187645)) ;
#10450 = CARTESIAN_POINT('Ctrl Pts',(-24.2238084309022,20.6992979967966,32.5665017098134)) ;
#10451 = CARTESIAN_POINT('Ctrl Pts',(-24.2090227178855,20.71057946702,32.5850854157313)) ;
#10452 = CARTESIAN_POINT('Ctrl Pts',(-24.1719510657226,20.7295683297316,32.6163598545375)) ;
#10453 = CARTESIAN_POINT('Ctrl Pts',(-24.150019848274,20.7370942674122,32.6287518975251)) ;
#10454 = CARTESIAN_POINT('Ctrl Pts',(-24.1018348748854,20.7473591548606,32.6456526691067)) ;
#10455 = CARTESIAN_POINT('Ctrl Pts',(-24.0760419567382,20.75,32.65)) ;
#10456 = CARTESIAN_POINT('Ctrl Pts',(-24.05,20.75,32.65)) ;
#10457 = CARTESIAN_POINT('Origin',(-24.05,43.2596418025572,-36.388001295162)) ;
#10458 = CARTESIAN_POINT('',(-24.25,43.2596418025572,-36.388001295162)) ;
#10459 = CARTESIAN_POINT('',(-24.05,43.4593732974275,-36.3983613123869)) ;
#10460 = CARTESIAN_POINT('Origin',(-24.05,21.6437725346931,34.0916800205589)) ;
#10461 = CARTESIAN_POINT('',(-24.25,19.75,33.9947419676037)) ;
#10462 = CARTESIAN_POINT('Origin',(-24.25,21.6437725346931,34.0916800205589)) ;
#10463 = CARTESIAN_POINT('Ctrl Pts',(-24.25,19.75,33.9947419676037)) ;
#10464 = CARTESIAN_POINT('Ctrl Pts',(-24.25,19.7510782785915,33.9947695469051)) ;
#10465 = CARTESIAN_POINT('Ctrl Pts',(-24.2499912798646,19.7521565392983,33.9947971375223)) ;
#10466 = CARTESIAN_POINT('Ctrl Pts',(-24.2495525067901,19.7792823248453,33.9954915308927)) ;
#10467 = CARTESIAN_POINT('Ctrl Pts',(-24.244045930543,19.8049989553455,33.9961569948495)) ;
#10468 = CARTESIAN_POINT('Ctrl Pts',(-24.2234830661828,19.8528694600569,33.9974077124504)) ;
#10469 = CARTESIAN_POINT('Ctrl Pts',(-24.2086245409041,19.8745668657937,33.997980931313)) ;
#10470 = CARTESIAN_POINT('Ctrl Pts',(-24.1714290071766,19.9110377740365,33.9989510216977)) ;
#10471 = CARTESIAN_POINT('Ctrl Pts',(-24.1494502192513,19.9254650423844,33.9993384812983)) ;
#10472 = CARTESIAN_POINT('Ctrl Pts',(-24.1014008539367,19.944999534253,33.9998644932132)) ;
#10473 = CARTESIAN_POINT('Ctrl Pts',(-24.0758210331691,19.95,34.)) ;
#10474 = CARTESIAN_POINT('Ctrl Pts',(-24.05,19.95,34.0000000000001)) ;
#10475 = CARTESIAN_POINT('Origin',(-24.05,19.75,10.512952685943)) ;
#10476 = CARTESIAN_POINT('',(-24.25,19.75,10.512952685943)) ;
#10477 = CARTESIAN_POINT('Origin',(-24.05,27.3698141664511,-1.38697145397653)) ;
#10478 = CARTESIAN_POINT('',(-24.05,23.15,2.55)) ;
#10479 = CARTESIAN_POINT('',(-24.25,23.2911535780143,2.69168913446027)) ;
#10480 = CARTESIAN_POINT('Ctrl Pts',(-24.05,23.15,2.55)) ;
#10481 = CARTESIAN_POINT('Ctrl Pts',(-24.0632701694843,23.1499886889779,2.55001131102213)) ;
#10482 = CARTESIAN_POINT('Ctrl Pts',(-24.0765399924101,23.1509143468025,2.55095959089099)) ;
#10483 = CARTESIAN_POINT('Ctrl Pts',(-24.0895481340208,23.1527585208895,2.55282638702233)) ;
#10484 = CARTESIAN_POINT('Ctrl Pts',(-24.1025532968563,23.1546022726734,2.55469275567017)) ;
#10485 = CARTESIAN_POINT('Ctrl Pts',(-24.1152962197139,23.1573640218908,2.55747712175156)) ;
#10486 = CARTESIAN_POINT('Ctrl Pts',(-24.1275260588054,23.1609891810431,2.56112489776775)) ;
#10487 = CARTESIAN_POINT('Ctrl Pts',(-24.1397534773072,23.164613622686,2.56477195179821)) ;
#10488 = CARTESIAN_POINT('Ctrl Pts',(-24.1514673780365,23.1691009417701,2.56928188326987)) ;
#10489 = CARTESIAN_POINT('Ctrl Pts',(-24.1624372641837,23.1743626179299,2.57456617181717)) ;
#10490 = CARTESIAN_POINT('Ctrl Pts',(-24.1734053194262,23.1796234159013,2.57984957840199)) ;
#10491 = CARTESIAN_POINT('Ctrl Pts',(-24.1836290375724,23.1856580368581,2.58590680797231)) ;
#10492 = CARTESIAN_POINT('Ctrl Pts',(-24.1929073111898,23.1923475533722,2.59261893309988)) ;
#10493 = CARTESIAN_POINT('Ctrl Pts',(-24.2021908572985,23.1990408712851,2.59933487247379)) ;
#10494 = CARTESIAN_POINT('Ctrl Pts',(-24.2105273961138,23.2063894818443,2.60670610449407)) ;
#10495 = CARTESIAN_POINT('Ctrl Pts',(-24.2177527569689,23.2142484468191,2.61458769092999)) ;
#10496 = CARTESIAN_POINT('Ctrl Pts',(-24.2249750808544,23.2221041085074,2.62246596457109)) ;
#10497 = CARTESIAN_POINT('Ctrl Pts',(-24.2310867869367,23.2304692838499,2.63085375186639)) ;
#10498 = CARTESIAN_POINT('Ctrl Pts',(-24.2359676185276,23.2391791534182,2.63958623338751)) ;
#10499 = CARTESIAN_POINT('Ctrl Pts',(-24.2408502551657,23.2478922441029,2.64832194438742)) ;
#10500 = CARTESIAN_POINT('Ctrl Pts',(-24.2445008489509,23.2569498295499,2.65740215014967)) ;
#10501 = CARTESIAN_POINT('Ctrl Pts',(-24.2468475163264,23.2661733348448,2.66664827575977)) ;
#10502 = CARTESIAN_POINT('Ctrl Pts',(-24.2489436334282,23.2744120598512,2.67490720594314)) ;
#10503 = CARTESIAN_POINT('Ctrl Pts',(-24.25,23.2827827492619,2.68329810053082)) ;
#10504 = CARTESIAN_POINT('Ctrl Pts',(-24.25,23.2911535780144,2.6916891344603)) ;
#10505 = CARTESIAN_POINT('',(-24.25,27.3698141664511,-1.38697145397653)) ;
#10506 = CARTESIAN_POINT('',(-24.05,27.2283928102138,-1.52839281021384)) ;
#10507 = CARTESIAN_POINT('Origin',(-24.05,17.2261159840305,33.8238840159695)) ;
#10508 = CARTESIAN_POINT('',(-24.25,17.1987235045028,33.2996639834704)) ;
#10509 = CARTESIAN_POINT('Origin',(-24.25,17.2261159840305,33.8238840159695)) ;
#10510 = CARTESIAN_POINT('Ctrl Pts',(-24.25,17.1987235045028,33.2996639834704)) ;
#10511 = CARTESIAN_POINT('Ctrl Pts',(-24.25,17.1987230610883,33.301013065151)) ;
#10512 = CARTESIAN_POINT('Ctrl Pts',(-24.2499863874771,17.1987227661361,33.3023621127686)) ;
#10513 = CARTESIAN_POINT('Ctrl Pts',(-24.2494407904293,17.1987198608847,33.3293950031184)) ;
#10514 = CARTESIAN_POINT('Ctrl Pts',(-24.2439924301409,17.1987735623143,33.3547437391131)) ;
#10515 = CARTESIAN_POINT('Ctrl Pts',(-24.2236773306868,17.1989855389576,33.4023588449877)) ;
#10516 = CARTESIAN_POINT('Ctrl Pts',(-24.2088610786989,17.1991433664022,33.4241220030844)) ;
#10517 = CARTESIAN_POINT('Ctrl Pts',(-24.1717621164808,17.199483617429,33.4607013743553)) ;
#10518 = CARTESIAN_POINT('Ctrl Pts',(-24.1498475303235,17.1996607603534,33.475185047544)) ;
#10519 = CARTESIAN_POINT('Ctrl Pts',(-24.1017273992471,17.199921556701,33.4949236590357)) ;
#10520 = CARTESIAN_POINT('Ctrl Pts',(-24.0759897994102,17.2,33.5)) ;
#10521 = CARTESIAN_POINT('Ctrl Pts',(-24.05,17.2,33.5)) ;
#10522 = CARTESIAN_POINT('Origin',(-24.05,20.3521649222088,3.15764237037056)) ;
#10523 = CARTESIAN_POINT('',(-24.25,18.2941489582325,11.498022857368)) ;
#10524 = CARTESIAN_POINT('',(-24.25,20.3521649222088,3.15764237037056)) ;
#10525 = CARTESIAN_POINT('',(-24.05,18.1,11.45)) ;
#10526 = CARTESIAN_POINT('Ctrl Pts',(-24.25,18.2941488864464,11.4980231468816)) ;
#10527 = CARTESIAN_POINT('Ctrl Pts',(-24.25,18.2931711440881,11.4977812986393)) ;
#10528 = CARTESIAN_POINT('Ctrl Pts',(-24.2499923914673,18.292193415111,11.4975394541043)) ;
#10529 = CARTESIAN_POINT('Ctrl Pts',(-24.2495857492044,18.2660672742236,11.491077053847)) ;
#10530 = CARTESIAN_POINT('Ctrl Pts',(-24.2441638802667,18.2412305566091,11.4849336180087)) ;
#10531 = CARTESIAN_POINT('Ctrl Pts',(-24.2238111338179,18.1948292452196,11.4734561374442)) ;
#10532 = CARTESIAN_POINT('Ctrl Pts',(-24.2090259631664,18.173725801069,11.4682361612198)) ;
#10533 = CARTESIAN_POINT('Ctrl Pts',(-24.1719547805075,18.1382083382914,11.4594508639049)) ;
#10534 = CARTESIAN_POINT('Ctrl Pts',(-24.1500231903924,18.1241338849213,11.4559695344032)) ;
#10535 = CARTESIAN_POINT('Ctrl Pts',(-24.1018369369122,18.104937954276,11.4512214053055)) ;
#10536 = CARTESIAN_POINT('Ctrl Pts',(-24.0760429610237,18.0999999999997,11.4500000000011)) ;
#10537 = CARTESIAN_POINT('Ctrl Pts',(-24.05,18.0999999999997,11.4500000000014)) ;
#10538 = CARTESIAN_POINT('',(-24.05,20.1579889903124,3.10972882873379)) ;
#10539 = CARTESIAN_POINT('Origin',(-24.05,36.5141483124065,16.0157526941183)) ;
#10540 = CARTESIAN_POINT('Origin',(-24.05,36.5141483124065,16.0157526941183)) ;
#10541 = CARTESIAN_POINT('Origin',(-24.25,36.5141483124065,16.0157526941183)) ;
#10542 = CARTESIAN_POINT('Origin',(-24.05,17.5172318824408,27.2801860892852)) ;
#10543 = CARTESIAN_POINT('',(-24.25,11.9761936845669,29.6534659706104)) ;
#10544 = CARTESIAN_POINT('Origin',(-24.25,17.5172318824408,27.2801860892852)) ;
#10545 = CARTESIAN_POINT('Ctrl Pts',(-24.25,11.976193684567,29.6534659706103)) ;
#10546 = CARTESIAN_POINT('Ctrl Pts',(-24.25,11.9755977818072,29.6537918503201)) ;
#10547 = CARTESIAN_POINT('Ctrl Pts',(-24.249996571899,11.9750018853708,29.6541177328252)) ;
#10548 = CARTESIAN_POINT('Ctrl Pts',(-24.2497216151694,11.9511052235039,29.6671865363954)) ;
#10549 = CARTESIAN_POINT('Ctrl Pts',(-24.2442143166798,11.9280772247116,29.67979017374)) ;
#10550 = CARTESIAN_POINT('Ctrl Pts',(-24.2235106312593,11.8855929764579,29.7030577904185)) ;
#10551 = CARTESIAN_POINT('Ctrl Pts',(-24.2086691696459,11.866481196583,29.7135326615679)) ;
#10552 = CARTESIAN_POINT('Ctrl Pts',(-24.1715506168807,11.8344052888093,29.7311205240322)) ;
#10553 = CARTESIAN_POINT('Ctrl Pts',(-24.1496614544952,11.8217190498113,29.7380808841414)) ;
#10554 = CARTESIAN_POINT('Ctrl Pts',(-24.1016151251543,11.8044416410205,29.7475617250063)) ;
#10555 = CARTESIAN_POINT('Ctrl Pts',(-24.0759347764714,11.8,29.75)) ;
#10556 = CARTESIAN_POINT('Ctrl Pts',(-24.05,11.8,29.75)) ;
#10557 = CARTESIAN_POINT('Origin',(-24.05,3.95376271603246,17.8309361222439)) ;
#10558 = CARTESIAN_POINT('',(-24.25,11.0061123301193,28.2238723956349)) ;
#10559 = CARTESIAN_POINT('',(-24.25,3.95376271603246,17.8309361222439)) ;
#10560 = CARTESIAN_POINT('Ctrl Pts',(-24.25,11.0061123301191,28.2238723956351)) ;
#10561 = CARTESIAN_POINT('Ctrl Pts',(-24.25,11.0055804043094,28.2243014934111)) ;
#10562 = CARTESIAN_POINT('Ctrl Pts',(-24.2499965208248,11.0050484851104,28.2247305924736)) ;
#10563 = CARTESIAN_POINT('Ctrl Pts',(-24.24971885402,10.9838233720669,28.24185314932)) ;
#10564 = CARTESIAN_POINT('Ctrl Pts',(-24.2441849834891,10.9633766729638,28.2583581483305)) ;
#10565 = CARTESIAN_POINT('Ctrl Pts',(-24.2234123635662,10.92570478066,28.2887842809354)) ;
#10566 = CARTESIAN_POINT('Ctrl Pts',(-24.2085470530348,10.908781248086,28.3024612708704)) ;
#10567 = CARTESIAN_POINT('Ctrl Pts',(-24.1713793201344,10.8803789404798,28.3254235047367)) ;
#10568 = CARTESIAN_POINT('Ctrl Pts',(-24.1494579257414,10.8691509765059,28.3345056873335)) ;
#10569 = CARTESIAN_POINT('Ctrl Pts',(-24.101449145542,10.8539092421029,28.3468363151276)) ;
#10570 = CARTESIAN_POINT('Ctrl Pts',(-24.0758491730085,10.85,28.35)) ;
#10571 = CARTESIAN_POINT('Ctrl Pts',(-24.05,10.85,28.35)) ;
#10572 = CARTESIAN_POINT('Origin',(-24.05,6.94557266623349,32.0941410006498)) ;
#10573 = CARTESIAN_POINT('',(-24.25,8.97014939515615,26.8626927780581)) ;
#10574 = CARTESIAN_POINT('Origin',(-24.25,6.94557266623349,32.0941410006498)) ;
#10575 = CARTESIAN_POINT('Ctrl Pts',(-24.25,8.97014939515615,26.8626927780581)) ;
#10576 = CARTESIAN_POINT('Ctrl Pts',(-24.25,8.96980308364487,26.8636177522324)) ;
#10577 = CARTESIAN_POINT('Ctrl Pts',(-24.2499926845694,8.96945677554181,26.8645427132223)) ;
#10578 = CARTESIAN_POINT('Ctrl Pts',(-24.2495939082893,8.96001834118659,26.8897518974775)) ;
#10579 = CARTESIAN_POINT('Ctrl Pts',(-24.2441704958547,8.95103756375155,26.9137357983753)) ;
#10580 = CARTESIAN_POINT('Ctrl Pts',(-24.2238069800194,8.93426601854433,26.9585208446484)) ;
#10581 = CARTESIAN_POINT('Ctrl Pts',(-24.2090209946366,8.92664079883623,26.9788799538848)) ;
#10582 = CARTESIAN_POINT('Ctrl Pts',(-24.1719491121253,8.91380708303496,27.0131430696368)) ;
#10583 = CARTESIAN_POINT('Ctrl Pts',(-24.1500181006065,8.90872114416501,27.0267199513304)) ;
#10584 = CARTESIAN_POINT('Ctrl Pts',(-24.1018338032566,8.90178447987708,27.0452368074564)) ;
#10585 = CARTESIAN_POINT('Ctrl Pts',(-24.0760414340743,8.90000000000021,27.0500000000001)) ;
#10586 = CARTESIAN_POINT('Ctrl Pts',(-24.05,8.9000000000002,27.0500000000001)) ;
#10587 = CARTESIAN_POINT('Origin',(-24.05,9.21323262385133,26.950665756062)) ;
#10588 = CARTESIAN_POINT('',(-24.25,3.70650846391516,24.9577560600852)) ;
#10589 = CARTESIAN_POINT('',(-24.25,9.21323262385133,26.950665756062)) ;
#10590 = CARTESIAN_POINT('Ctrl Pts',(-24.25,3.70650846391515,24.9577560600852)) ;
#10591 = CARTESIAN_POINT('Ctrl Pts',(-24.25,3.70613263983912,24.9591249412748)) ;
#10592 = CARTESIAN_POINT('Ctrl Pts',(-24.2499849817197,3.70575595542866,24.9604935443132)) ;
#10593 = CARTESIAN_POINT('Ctrl Pts',(-24.249412424472,3.69856163593084,24.9865707375015)) ;
#10594 = CARTESIAN_POINT('Ctrl Pts',(-24.243975112071,3.69157540066717,25.0108789195625)) ;
#10595 = CARTESIAN_POINT('Ctrl Pts',(-24.2237007313829,3.67823129499148,25.0565205811117)) ;
#10596 = CARTESIAN_POINT('Ctrl Pts',(-24.2089065576862,3.67201058953836,25.0773585750523)) ;
#10597 = CARTESIAN_POINT('Ctrl Pts',(-24.1718321061545,3.66147275373824,25.1123866592332)) ;
#10598 = CARTESIAN_POINT('Ctrl Pts',(-24.1499165688336,3.65725415494464,25.1262472800193)) ;
#10599 = CARTESIAN_POINT('Ctrl Pts',(-24.1017741331367,3.65149079158464,25.1451425855635)) ;
#10600 = CARTESIAN_POINT('Ctrl Pts',(-24.0760121197655,3.64999999999993,25.15)) ;
#10601 = CARTESIAN_POINT('Ctrl Pts',(-24.05,3.64999999999994,25.15)) ;
#10602 = CARTESIAN_POINT('Ctrl Pts',(-24.25,3.70650846391516,24.9577560600852)) ;
#10603 = CARTESIAN_POINT('Ctrl Pts',(-24.25,3.58356237630651,24.9342829362711)) ;
#10604 = CARTESIAN_POINT('Ctrl Pts',(-24.25,3.6,24.8102001714438)) ;
#10605 = CARTESIAN_POINT('Ctrl Pts',(-24.25,3.66900151529777,25.1542076541367)) ;
#10606 = CARTESIAN_POINT('Ctrl Pts',(-24.25,3.36048403150656,25.0953048518053)) ;
#10607 = CARTESIAN_POINT('Ctrl Pts',(-24.25,3.40173214602618,24.7839350218989)) ;
#10608 = CARTESIAN_POINT('Ctrl Pts',(-24.05,3.66900151529777,25.1542076541367)) ;
#10609 = CARTESIAN_POINT('Ctrl Pts',(-24.05,3.36048403150656,25.0953048518053)) ;
#10610 = CARTESIAN_POINT('Ctrl Pts',(-24.05,3.40173214602618,24.7839350218989)) ;
#10611 = CARTESIAN_POINT('',(-24.25,3.6,24.8102001714438)) ;
#10612 = CARTESIAN_POINT('Origin',(-24.25,3.73135783556136,24.8276015460276)) ;
#10613 = CARTESIAN_POINT('Ctrl Pts',(-24.25,3.6,24.8102001714438)) ;
#10614 = CARTESIAN_POINT('Ctrl Pts',(-24.25,3.59858329627815,24.8101067420225)) ;
#10615 = CARTESIAN_POINT('Ctrl Pts',(-24.2499849471218,3.59716658347762,24.8100140642959)) ;
#10616 = CARTESIAN_POINT('Ctrl Pts',(-24.2494121494215,3.57021683344487,24.8082647222741)) ;
#10617 = CARTESIAN_POINT('Ctrl Pts',(-24.2439829942548,3.54500851791206,24.8068523074975)) ;
#10618 = CARTESIAN_POINT('Ctrl Pts',(-24.2237349857366,3.49756309113979,24.8043748002524)) ;
#10619 = CARTESIAN_POINT('Ctrl Pts',(-24.2089435980113,3.4758431175171,24.8033431470145)) ;
#10620 = CARTESIAN_POINT('Ctrl Pts',(-24.1718701468162,3.43929965309513,24.801671969686)) ;
#10621 = CARTESIAN_POINT('Ctrl Pts',(-24.1499496297251,3.42482149959621,24.8010487344218)) ;
#10622 = CARTESIAN_POINT('Ctrl Pts',(-24.1017936039468,3.40507852591201,24.8002087457528)) ;
#10623 = CARTESIAN_POINT('Ctrl Pts',(-24.0760216817082,3.4,24.8)) ;
#10624 = CARTESIAN_POINT('Ctrl Pts',(-24.05,3.4,24.8)) ;
#10625 = CARTESIAN_POINT('Origin',(-24.05,3.6,5.91295268594296)) ;
#10626 = CARTESIAN_POINT('',(-24.25,3.6,5.91295268594296)) ;
#10627 = CARTESIAN_POINT('Origin',(-24.25,3.9,19.5)) ;
#10628 = CARTESIAN_POINT('',(-24.25,10.8,22.)) ;
#10629 = CARTESIAN_POINT('Origin',(-24.25,12.2182755082439,18.0689260404997)) ;
#10630 = CARTESIAN_POINT('',(-24.25,12.85,22.2)) ;
#10631 = CARTESIAN_POINT('Origin',(-24.25,12.85,22.2)) ;
#10632 = CARTESIAN_POINT('',(-24.25,15.5,20.65)) ;
#10633 = CARTESIAN_POINT('Origin',(-24.25,12.5256959686759,18.3486581187154)) ;
#10634 = CARTESIAN_POINT('',(-24.25,16.2,19.15)) ;
#10635 = CARTESIAN_POINT('Origin',(-24.25,16.2,19.15)) ;
#10636 = CARTESIAN_POINT('',(-24.25,18.1,11.45)) ;
#10637 = CARTESIAN_POINT('Origin',(-24.25,36.5141483124065,16.0157526941183)) ;
#10638 = CARTESIAN_POINT('',(-24.25,23.15,2.55)) ;
#10639 = CARTESIAN_POINT('Origin',(-24.25,23.15,2.55)) ;
#10640 = CARTESIAN_POINT('',(-24.25,35.4,-9.7)) ;
#10641 = CARTESIAN_POINT('Origin',(-24.25,29.7633733578399,-15.291248496029)) ;
#10642 = CARTESIAN_POINT('',(-24.25,37.7,-15.5)) ;
#10643 = CARTESIAN_POINT('Origin',(-24.25,37.7,-15.5)) ;
#10644 = CARTESIAN_POINT('',(-24.25,36.65,-56.2)) ;
#10645 = CARTESIAN_POINT('Origin',(-24.25,37.7318176617063,-60.502128268216)) ;
#10646 = CARTESIAN_POINT('',(-24.25,42.15,-60.9)) ;
#10647 = CARTESIAN_POINT('Origin',(-24.25,42.15,-60.9)) ;
#10648 = CARTESIAN_POINT('',(-24.25,42.3,-58.75)) ;
#10649 = CARTESIAN_POINT('Origin',(-24.25,42.3,-58.75)) ;
#10650 = CARTESIAN_POINT('',(-24.25,44.45,-17.3)) ;
#10651 = CARTESIAN_POINT('Origin',(-24.25,23.7122919887408,-16.1822567109578)) ;
#10652 = CARTESIAN_POINT('',(-24.25,38.35,-1.45)) ;
#10653 = CARTESIAN_POINT('Origin',(-24.25,38.35,-1.45)) ;
#10654 = CARTESIAN_POINT('Origin',(-24.25,23.9394766127413,-12.9740946281141)) ;
#10655 = CARTESIAN_POINT('',(-24.25,19.6,36.797821691004)) ;
#10656 = CARTESIAN_POINT('',(-24.25,17.9,36.797821691004)) ;
#10657 = CARTESIAN_POINT('Origin',(-24.25,18.75,36.8151771653543)) ;
#10658 = CARTESIAN_POINT('',(-24.25,19.6,37.802178308996)) ;
#10659 = CARTESIAN_POINT('',(-24.25,19.6,12.412952685943)) ;
#10660 = CARTESIAN_POINT('',(-24.25,17.9,37.802178308996)) ;
#10661 = CARTESIAN_POINT('Origin',(-24.25,18.75,37.7848228346457)) ;
#10662 = CARTESIAN_POINT('',(-24.25,17.9,11.912952685943)) ;
#10663 = CARTESIAN_POINT('',(-24.25,17.565,31.11)) ;
#10664 = CARTESIAN_POINT('Origin',(-24.25,17.565,27.14)) ;
#10665 = CARTESIAN_POINT('Origin',(-16.5,19.6,12.412952685943)) ;
#10666 = CARTESIAN_POINT('',(-16.5,19.4,37.8)) ;
#10667 = CARTESIAN_POINT('Ctrl Pts',(-16.3,19.6,37.802178308996)) ;
#10668 = CARTESIAN_POINT('Ctrl Pts',(-16.3,19.5980557067222,37.8021584615749)) ;
#10669 = CARTESIAN_POINT('Ctrl Pts',(-16.3000283520726,19.5961115171112,37.8021385811547)) ;
#10670 = CARTESIAN_POINT('Ctrl Pts',(-16.3008130702058,19.5692119515023,37.8018630425845)) ;
#10671 = CARTESIAN_POINT('Ctrl Pts',(-16.3062077376902,19.544611369092,37.8016051814373)) ;
#10672 = CARTESIAN_POINT('Ctrl Pts',(-16.3261931704212,19.4976798310454,37.8011023681781)) ;
#10673 = CARTESIAN_POINT('Ctrl Pts',(-16.3409792801415,19.4759408829566,37.8008632966273)) ;
#10674 = CARTESIAN_POINT('Ctrl Pts',(-16.378051291451,19.4393554460034,37.8004539917046)) ;
#10675 = CARTESIAN_POINT('Ctrl Pts',(-16.3999823105663,19.4248582008503,37.8002878723196)) ;
#10676 = CARTESIAN_POINT('Ctrl Pts',(-16.4481664789317,19.4050861143264,37.8000596824773)) ;
#10677 = CARTESIAN_POINT('Ctrl Pts',(-16.4739586994907,19.4,37.8)) ;
#10678 = CARTESIAN_POINT('Ctrl Pts',(-16.5,19.4,37.8)) ;
#10679 = CARTESIAN_POINT('',(-16.5,19.4,36.8)) ;
#10680 = CARTESIAN_POINT('',(-16.5,19.4,12.412952685943)) ;
#10681 = CARTESIAN_POINT('Ctrl Pts',(-16.3,19.6,36.797821691004)) ;
#10682 = CARTESIAN_POINT('Ctrl Pts',(-16.3,19.5980557067222,36.797841538425)) ;
#10683 = CARTESIAN_POINT('Ctrl Pts',(-16.3000283520726,19.5961115171112,36.7978614188453)) ;
#10684 = CARTESIAN_POINT('Ctrl Pts',(-16.3008130702058,19.5692119515023,36.7981369574155)) ;
#10685 = CARTESIAN_POINT('Ctrl Pts',(-16.3062077376902,19.544611369092,36.7983948185627)) ;
#10686 = CARTESIAN_POINT('Ctrl Pts',(-16.3261931704212,19.4976798310454,36.7988976318219)) ;
#10687 = CARTESIAN_POINT('Ctrl Pts',(-16.3409792801416,19.4759408829566,36.7991367033726)) ;
#10688 = CARTESIAN_POINT('Ctrl Pts',(-16.3780512914511,19.4393554460034,36.7995460082953)) ;
#10689 = CARTESIAN_POINT('Ctrl Pts',(-16.3999823105663,19.4248582008503,36.7997121276805)) ;
#10690 = CARTESIAN_POINT('Ctrl Pts',(-16.4481664789317,19.4050861143264,36.7999403175228)) ;
#10691 = CARTESIAN_POINT('Ctrl Pts',(-16.4739586994907,19.4,36.8)) ;
#10692 = CARTESIAN_POINT('Ctrl Pts',(-16.5,19.4,36.8)) ;
#10693 = CARTESIAN_POINT('Origin',(-16.5,18.75,37.7848228346457)) ;
#10694 = CARTESIAN_POINT('',(-16.5,18.1,37.8)) ;
#10695 = CARTESIAN_POINT('Ctrl Pts',(-16.3,17.9,37.8021783089959)) ;
#10696 = CARTESIAN_POINT('Ctrl Pts',(-16.3,17.9019442932778,37.8021584615748)) ;
#10697 = CARTESIAN_POINT('Ctrl Pts',(-16.3000283520726,17.9038884828888,37.8021385811547)) ;
#10698 = CARTESIAN_POINT('Ctrl Pts',(-16.3008130702058,17.9307880484977,37.8018630425845)) ;
#10699 = CARTESIAN_POINT('Ctrl Pts',(-16.3062077376903,17.9553886309081,37.8016051814374)) ;
#10700 = CARTESIAN_POINT('Ctrl Pts',(-16.3261931704213,18.0023201689547,37.8011023681781)) ;
#10701 = CARTESIAN_POINT('Ctrl Pts',(-16.3409792801416,18.0240591170434,37.8008632966274)) ;
#10702 = CARTESIAN_POINT('Ctrl Pts',(-16.3780512914511,18.0606445539966,37.8004539917047)) ;
#10703 = CARTESIAN_POINT('Ctrl Pts',(-16.3999823105663,18.0751417991497,37.8002878723196)) ;
#10704 = CARTESIAN_POINT('Ctrl Pts',(-16.4481664789317,18.0949138856736,37.8000596824773)) ;
#10705 = CARTESIAN_POINT('Ctrl Pts',(-16.4739586994907,18.1,37.8)) ;
#10706 = CARTESIAN_POINT('Ctrl Pts',(-16.5,18.1,37.8)) ;
#10707 = CARTESIAN_POINT('Origin',(-16.5,18.75,37.7848228346457)) ;
#10708 = CARTESIAN_POINT('Origin',(-16.5,17.9,11.912952685943)) ;
#10709 = CARTESIAN_POINT('',(-16.5,18.1,36.8)) ;
#10710 = CARTESIAN_POINT('Ctrl Pts',(-16.3,17.9,36.797821691004)) ;
#10711 = CARTESIAN_POINT('Ctrl Pts',(-16.3,17.9019442932778,36.7978415384251)) ;
#10712 = CARTESIAN_POINT('Ctrl Pts',(-16.3000283520726,17.9038884828888,36.7978614188453)) ;
#10713 = CARTESIAN_POINT('Ctrl Pts',(-16.3008130702058,17.9307880484976,36.7981369574155)) ;
#10714 = CARTESIAN_POINT('Ctrl Pts',(-16.3062077376902,17.955388630908,36.7983948185627)) ;
#10715 = CARTESIAN_POINT('Ctrl Pts',(-16.3261931704212,18.0023201689546,36.7988976318219)) ;
#10716 = CARTESIAN_POINT('Ctrl Pts',(-16.3409792801416,18.0240591170434,36.7991367033726)) ;
#10717 = CARTESIAN_POINT('Ctrl Pts',(-16.3780512914511,18.0606445539966,36.7995460082953)) ;
#10718 = CARTESIAN_POINT('Ctrl Pts',(-16.3999823105663,18.0751417991497,36.7997121276805)) ;
#10719 = CARTESIAN_POINT('Ctrl Pts',(-16.4481664789317,18.0949138856736,36.7999403175228)) ;
#10720 = CARTESIAN_POINT('Ctrl Pts',(-16.4739586994907,18.1,36.8)) ;
#10721 = CARTESIAN_POINT('Ctrl Pts',(-16.5,18.1,36.8)) ;
#10722 = CARTESIAN_POINT('',(-16.5,18.1,11.912952685943)) ;
#10723 = CARTESIAN_POINT('Origin',(-16.5,18.75,36.8151771653543)) ;
#10724 = CARTESIAN_POINT('Origin',(-16.5,18.75,36.8151771653543)) ;
#10725 = CARTESIAN_POINT('Origin',(-24.25,18.75,36.8151771653543)) ;
#10726 = CARTESIAN_POINT('',(-24.05,19.4,36.8)) ;
#10727 = CARTESIAN_POINT('',(-24.25,19.4,36.8)) ;
#10728 = CARTESIAN_POINT('',(-24.05,18.1,36.8)) ;
#10729 = CARTESIAN_POINT('Origin',(-24.05,18.75,36.8151771653543)) ;
#10730 = CARTESIAN_POINT('',(-24.25,18.1,36.8)) ;
#10731 = CARTESIAN_POINT('Origin',(-24.25,19.4,37.8)) ;
#10732 = CARTESIAN_POINT('',(-24.05,19.4,37.8)) ;
#10733 = CARTESIAN_POINT('',(-24.25,19.4,37.8)) ;
#10734 = CARTESIAN_POINT('',(-24.05,19.4,12.412952685943)) ;
#10735 = CARTESIAN_POINT('Origin',(-24.05,18.75,37.7848228346457)) ;
#10736 = CARTESIAN_POINT('',(-24.05,18.1,37.8)) ;
#10737 = CARTESIAN_POINT('Origin',(-24.05,18.75,37.7848228346457)) ;
#10738 = CARTESIAN_POINT('Ctrl Pts',(-24.05,18.1,37.8)) ;
#10739 = CARTESIAN_POINT('Ctrl Pts',(-24.0760413005093,18.1,37.8)) ;
#10740 = CARTESIAN_POINT('Ctrl Pts',(-24.1018335210683,18.0949138856736,37.8000596824775)) ;
#10741 = CARTESIAN_POINT('Ctrl Pts',(-24.1500176894337,18.0751417991497,37.8002878723198)) ;
#10742 = CARTESIAN_POINT('Ctrl Pts',(-24.171948708549,18.0606445539966,37.8004539917047)) ;
#10743 = CARTESIAN_POINT('Ctrl Pts',(-24.2090207198584,18.0240591170434,37.8008632966275)) ;
#10744 = CARTESIAN_POINT('Ctrl Pts',(-24.2238068295788,18.0023201689546,37.801102368178)) ;
#10745 = CARTESIAN_POINT('Ctrl Pts',(-24.2437922623098,17.9553886309081,37.8016051814372)) ;
#10746 = CARTESIAN_POINT('Ctrl Pts',(-24.2491869297942,17.9307880484976,37.8018630425845)) ;
#10747 = CARTESIAN_POINT('Ctrl Pts',(-24.2499716479274,17.9038884828888,37.8021385811547)) ;
#10748 = CARTESIAN_POINT('Ctrl Pts',(-24.25,17.9019442932778,37.8021584615749)) ;
#10749 = CARTESIAN_POINT('Ctrl Pts',(-24.25,17.9,37.802178308996)) ;
#10750 = CARTESIAN_POINT('Ctrl Pts',(-24.25,19.6,37.802178308996)) ;
#10751 = CARTESIAN_POINT('Ctrl Pts',(-24.25,19.5980557067222,37.8021584615749)) ;
#10752 = CARTESIAN_POINT('Ctrl Pts',(-24.2499716479274,19.5961115171112,37.8021385811546)) ;
#10753 = CARTESIAN_POINT('Ctrl Pts',(-24.2491869297942,19.5692119515024,37.8018630425845)) ;
#10754 = CARTESIAN_POINT('Ctrl Pts',(-24.2437922623098,19.5446113690919,37.801605181438)) ;
#10755 = CARTESIAN_POINT('Ctrl Pts',(-24.2238068295787,19.4976798310453,37.8011023681784)) ;
#10756 = CARTESIAN_POINT('Ctrl Pts',(-24.2090207198584,19.4759408829566,37.8008632966275)) ;
#10757 = CARTESIAN_POINT('Ctrl Pts',(-24.171948708549,19.4393554460034,37.8004539917047)) ;
#10758 = CARTESIAN_POINT('Ctrl Pts',(-24.1500176894337,19.4248582008503,37.8002878723198)) ;
#10759 = CARTESIAN_POINT('Ctrl Pts',(-24.1018335210683,19.4050861143264,37.8000596824775)) ;
#10760 = CARTESIAN_POINT('Ctrl Pts',(-24.0760413005093,19.4,37.8)) ;
#10761 = CARTESIAN_POINT('Ctrl Pts',(-24.05,19.4,37.8)) ;
#10762 = CARTESIAN_POINT('Origin',(-24.05,18.75,36.8151771653543)) ;
#10763 = CARTESIAN_POINT('Ctrl Pts',(-24.25,17.9,36.797821691004)) ;
#10764 = CARTESIAN_POINT('Ctrl Pts',(-24.25,17.9019442932778,36.7978415384251)) ;
#10765 = CARTESIAN_POINT('Ctrl Pts',(-24.2499716479274,17.9038884828888,36.7978614188453)) ;
#10766 = CARTESIAN_POINT('Ctrl Pts',(-24.2491869297942,17.9307880484977,36.7981369574155)) ;
#10767 = CARTESIAN_POINT('Ctrl Pts',(-24.2437922623098,17.9553886309081,36.7983948185627)) ;
#10768 = CARTESIAN_POINT('Ctrl Pts',(-24.2238068295788,18.0023201689546,36.798897631822)) ;
#10769 = CARTESIAN_POINT('Ctrl Pts',(-24.2090207198584,18.0240591170434,36.7991367033725)) ;
#10770 = CARTESIAN_POINT('Ctrl Pts',(-24.171948708549,18.0606445539966,36.7995460082953)) ;
#10771 = CARTESIAN_POINT('Ctrl Pts',(-24.1500176894337,18.0751417991497,36.7997121276803)) ;
#10772 = CARTESIAN_POINT('Ctrl Pts',(-24.1018335210683,18.0949138856736,36.7999403175226)) ;
#10773 = CARTESIAN_POINT('Ctrl Pts',(-24.0760413005093,18.1,36.8)) ;
#10774 = CARTESIAN_POINT('Ctrl Pts',(-24.05,18.1,36.8)) ;
#10775 = CARTESIAN_POINT('Ctrl Pts',(-24.25,19.6,36.797821691004)) ;
#10776 = CARTESIAN_POINT('Ctrl Pts',(-24.25,19.5980557067222,36.7978415384251)) ;
#10777 = CARTESIAN_POINT('Ctrl Pts',(-24.2499716479274,19.5961115171112,36.7978614188453)) ;
#10778 = CARTESIAN_POINT('Ctrl Pts',(-24.2491869297942,19.5692119515023,36.7981369574155)) ;
#10779 = CARTESIAN_POINT('Ctrl Pts',(-24.2437922623098,19.5446113690919,36.7983948185627)) ;
#10780 = CARTESIAN_POINT('Ctrl Pts',(-24.2238068295788,19.4976798310454,36.798897631822)) ;
#10781 = CARTESIAN_POINT('Ctrl Pts',(-24.2090207198584,19.4759408829566,36.7991367033725)) ;
#10782 = CARTESIAN_POINT('Ctrl Pts',(-24.171948708549,19.4393554460034,36.7995460082953)) ;
#10783 = CARTESIAN_POINT('Ctrl Pts',(-24.1500176894337,19.4248582008503,36.7997121276803)) ;
#10784 = CARTESIAN_POINT('Ctrl Pts',(-24.1018335210683,19.4050861143264,36.7999403175226)) ;
#10785 = CARTESIAN_POINT('Ctrl Pts',(-24.0760413005093,19.4,36.8)) ;
#10786 = CARTESIAN_POINT('Ctrl Pts',(-24.05,19.4,36.8)) ;
#10787 = CARTESIAN_POINT('Origin',(-24.05,17.9,11.912952685943)) ;
#10788 = CARTESIAN_POINT('',(-24.05,18.1,11.912952685943)) ;
#10789 = CARTESIAN_POINT('Origin',(-24.05,19.6,12.412952685943)) ;
#10790 = CARTESIAN_POINT('Origin',(-24.25,17.565,27.14)) ;
#10791 = CARTESIAN_POINT('',(-24.25,17.565,31.11)) ;
#10792 = CARTESIAN_POINT('Origin',(-24.25,18.1,36.8)) ;
#10793 = CARTESIAN_POINT('',(-24.25,18.1,37.8)) ;
#10794 = CARTESIAN_POINT('Origin',(-24.25,18.75,37.7848228346457)) ;
#10795 = CARTESIAN_POINT('',(0.,0.,0.)) ;
#10796 = CARTESIAN_POINT('Origin',(-27.15,21.265,27.14)) ;
#10797 = CARTESIAN_POINT('',(-27.15,13.865,27.14)) ;
#10798 = CARTESIAN_POINT('Origin',(-27.15,17.565,27.14)) ;
#10799 = CARTESIAN_POINT('Origin',(-27.025,17.565,27.14)) ;
#10800 = CARTESIAN_POINT('',(-26.9,13.615,27.14)) ;
#10801 = CARTESIAN_POINT('Origin',(-26.9,17.565,27.14)) ;
#10802 = CARTESIAN_POINT('',(-27.025,13.74,27.14)) ;
#10803 = CARTESIAN_POINT('Origin',(-7.87,17.565,27.14)) ;
#10804 = CARTESIAN_POINT('',(11.16,13.615,27.14)) ;
#10805 = CARTESIAN_POINT('Origin',(11.16,17.565,27.14)) ;
#10806 = CARTESIAN_POINT('',(-7.87,13.615,27.14)) ;
#10807 = CARTESIAN_POINT('Origin',(11.285,17.565,27.14)) ;
#10808 = CARTESIAN_POINT('',(11.41,13.865,27.14)) ;
#10809 = CARTESIAN_POINT('Origin',(11.41,17.565,27.14)) ;
#10810 = CARTESIAN_POINT('',(11.285,13.74,27.14)) ;
#10811 = CARTESIAN_POINT('Origin',(11.41,17.565,27.14)) ;
#10812 = CARTESIAN_POINT('',(0.,0.,0.)) ;
#10813 = CARTESIAN_POINT('Origin',(-9.76,21.29,38.695)) ;
#10814 = CARTESIAN_POINT('',(-9.76,18.29,38.695)) ;
#10815 = CARTESIAN_POINT('Origin',(-9.76,19.79,38.695)) ;
#10816 = CARTESIAN_POINT('Origin',(-8.005,19.79,38.695)) ;
#10817 = CARTESIAN_POINT('',(-6.25,18.29,38.695)) ;
#10818 = CARTESIAN_POINT('Origin',(-6.25,19.79,38.695)) ;
#10819 = CARTESIAN_POINT('',(-8.005,18.29,38.695)) ;
#10820 = CARTESIAN_POINT('Origin',(-6.25,24.715,38.695)) ;
#10821 = CARTESIAN_POINT('',(-6.25,14.865,38.695)) ;
#10822 = CARTESIAN_POINT('Origin',(-6.25,19.79,38.695)) ;
#10823 = CARTESIAN_POINT('Origin',(-6.125,19.79,38.695)) ;
#10824 = CARTESIAN_POINT('',(-6.,14.615,38.695)) ;
#10825 = CARTESIAN_POINT('Origin',(-6.,19.79,38.695)) ;
#10826 = CARTESIAN_POINT('',(-6.125,14.74,38.695)) ;
#10827 = CARTESIAN_POINT('Origin',(0.,19.79,38.695)) ;
#10828 = CARTESIAN_POINT('',(6.,14.615,38.695)) ;
#10829 = CARTESIAN_POINT('Origin',(6.,19.79,38.695)) ;
#10830 = CARTESIAN_POINT('',(0.,14.615,38.695)) ;
#10831 = CARTESIAN_POINT('Origin',(6.125,19.79,38.695)) ;
#10832 = CARTESIAN_POINT('',(6.25,14.865,38.695)) ;
#10833 = CARTESIAN_POINT('Origin',(6.25,19.79,38.695)) ;
#10834 = CARTESIAN_POINT('',(6.125,14.74,38.695)) ;
#10835 = CARTESIAN_POINT('Origin',(6.25,21.29,38.695)) ;
#10836 = CARTESIAN_POINT('',(6.25,18.29,38.695)) ;
#10837 = CARTESIAN_POINT('Origin',(6.25,19.79,38.695)) ;
#10838 = CARTESIAN_POINT('Origin',(8.005,19.79,38.695)) ;
#10839 = CARTESIAN_POINT('',(9.76,18.29,38.695)) ;
#10840 = CARTESIAN_POINT('Origin',(9.76,19.79,38.695)) ;
#10841 = CARTESIAN_POINT('',(8.005,18.29,38.695)) ;
#10842 = CARTESIAN_POINT('Origin',(9.76,19.79,38.695)) ;
#10843 = CARTESIAN_POINT('',(0.,0.,0.)) ;
#10844 = CARTESIAN_POINT('Origin',(1.875,7.535,-26.18)) ;
#10845 = CARTESIAN_POINT('',(-0.924999999999999,7.535,-26.18)) ;
#10846 = CARTESIAN_POINT('Origin',(0.475,7.535,-26.18)) ;
#10847 = CARTESIAN_POINT('Origin',(0.475,7.535,-26.055)) ;
#10848 = CARTESIAN_POINT('',(-1.175,7.535,-25.93)) ;
#10849 = CARTESIAN_POINT('Origin',(0.475,7.535,-25.93)) ;
#10850 = CARTESIAN_POINT('',(-1.05,7.535,-26.055)) ;
#10851 = CARTESIAN_POINT('Origin',(0.475,7.535,-3.895)) ;
#10852 = CARTESIAN_POINT('',(-1.175,7.535,18.14)) ;
#10853 = CARTESIAN_POINT('Origin',(0.475,7.535,18.14)) ;
#10854 = CARTESIAN_POINT('',(-1.175,7.535,-3.895)) ;
#10855 = CARTESIAN_POINT('Origin',(0.475,7.535,18.265)) ;
#10856 = CARTESIAN_POINT('',(-0.925,7.535,18.39)) ;
#10857 = CARTESIAN_POINT('Origin',(0.475,7.535,18.39)) ;
#10858 = CARTESIAN_POINT('',(-1.05,7.535,18.265)) ;
#10859 = CARTESIAN_POINT('Origin',(0.475,7.535,18.39)) ;
#10860 = CARTESIAN_POINT('',(0.,0.,0.)) ;
#10861 = CARTESIAN_POINT('Origin',(0.475,7.535,12.71)) ;
#10862 = CARTESIAN_POINT('',(-1.225,7.535,14.5)) ;
#10863 = CARTESIAN_POINT('Origin',(0.475,7.535,14.5)) ;
#10864 = CARTESIAN_POINT('',(-1.225,7.535,12.71)) ;
#10865 = CARTESIAN_POINT('',(-1.225,7.535,12.71)) ;
#10866 = CARTESIAN_POINT('Origin',(0.475,7.535,12.71)) ;
#10867 = CARTESIAN_POINT('Origin',(4.85,13.25,12.71)) ;
#10868 = CARTESIAN_POINT('',(4.85,13.25,12.71)) ;
#10869 = CARTESIAN_POINT('',(-4.05,13.55,12.71)) ;
#10870 = CARTESIAN_POINT('',(4.85,13.25,12.71)) ;
#10871 = CARTESIAN_POINT('',(-4.05,13.55,14.5)) ;
#10872 = CARTESIAN_POINT('',(-4.05,13.55,12.71)) ;
#10873 = CARTESIAN_POINT('',(4.85,13.25,14.5)) ;
#10874 = CARTESIAN_POINT('',(4.85,13.25,14.5)) ;
#10875 = CARTESIAN_POINT('',(4.85,13.25,12.71)) ;
#10876 = CARTESIAN_POINT('Origin',(5.3,9.9,12.71)) ;
#10877 = CARTESIAN_POINT('',(5.3,9.9,12.71)) ;
#10878 = CARTESIAN_POINT('',(5.3,9.9,12.71)) ;
#10879 = CARTESIAN_POINT('',(5.3,9.9,14.5)) ;
#10880 = CARTESIAN_POINT('',(5.3,9.9,14.5)) ;
#10881 = CARTESIAN_POINT('',(5.3,9.9,12.71)) ;
#10882 = CARTESIAN_POINT('Origin',(5.3,4.2,12.71)) ;
#10883 = CARTESIAN_POINT('',(5.3,4.2,12.71)) ;
#10884 = CARTESIAN_POINT('',(5.3,4.2,12.71)) ;
#10885 = CARTESIAN_POINT('',(5.3,4.2,14.5)) ;
#10886 = CARTESIAN_POINT('',(5.3,4.2,14.5)) ;
#10887 = CARTESIAN_POINT('',(5.3,4.2,12.71)) ;
#10888 = CARTESIAN_POINT('Origin',(5.2,4.15,12.71)) ;
#10889 = CARTESIAN_POINT('',(5.2,4.15,12.71)) ;
#10890 = CARTESIAN_POINT('',(5.2,4.15,12.71)) ;
#10891 = CARTESIAN_POINT('',(5.2,4.15,14.5)) ;
#10892 = CARTESIAN_POINT('',(5.2,4.15,14.5)) ;
#10893 = CARTESIAN_POINT('',(5.2,4.15,12.71)) ;
#10894 = CARTESIAN_POINT('Origin',(-0.6,4.2,12.71)) ;
#10895 = CARTESIAN_POINT('',(-0.6,4.2,12.71)) ;
#10896 = CARTESIAN_POINT('',(-0.6,4.2,12.71)) ;
#10897 = CARTESIAN_POINT('',(-0.6,4.2,14.5)) ;
#10898 = CARTESIAN_POINT('',(-0.6,4.2,14.5)) ;
#10899 = CARTESIAN_POINT('',(-0.6,4.2,12.71)) ;
#10900 = CARTESIAN_POINT('Origin',(-4.2,4.75,12.71)) ;
#10901 = CARTESIAN_POINT('',(-4.2,4.75,12.71)) ;
#10902 = CARTESIAN_POINT('',(-4.2,4.75,12.71)) ;
#10903 = CARTESIAN_POINT('',(-4.2,4.75,14.5)) ;
#10904 = CARTESIAN_POINT('',(-4.2,4.75,14.5)) ;
#10905 = CARTESIAN_POINT('',(-4.2,4.75,12.71)) ;
#10906 = CARTESIAN_POINT('Origin',(-4.25,5.5,12.71)) ;
#10907 = CARTESIAN_POINT('',(-4.25,5.5,12.71)) ;
#10908 = CARTESIAN_POINT('',(-4.25,5.5,12.71)) ;
#10909 = CARTESIAN_POINT('',(-4.25,5.5,14.5)) ;
#10910 = CARTESIAN_POINT('',(-4.25,5.5,14.5)) ;
#10911 = CARTESIAN_POINT('',(-4.25,5.5,12.71)) ;
#10912 = CARTESIAN_POINT('Origin',(-4.25,11.3,12.71)) ;
#10913 = CARTESIAN_POINT('',(-4.25,11.3,12.71)) ;
#10914 = CARTESIAN_POINT('',(-4.25,11.3,12.71)) ;
#10915 = CARTESIAN_POINT('',(-4.25,11.3,14.5)) ;
#10916 = CARTESIAN_POINT('',(-4.25,11.3,14.5)) ;
#10917 = CARTESIAN_POINT('',(-4.25,11.3,12.71)) ;
#10918 = CARTESIAN_POINT('Origin',(-4.05,13.55,12.71)) ;
#10919 = CARTESIAN_POINT('',(-4.05,13.55,12.71)) ;
#10920 = CARTESIAN_POINT('',(-4.05,13.55,14.5)) ;
#10921 = CARTESIAN_POINT('Origin',(0.525,8.85,14.5)) ;
#10922 = CARTESIAN_POINT('Origin',(0.525,8.85,12.71)) ;
#10923 = CARTESIAN_POINT('',(0.,0.,0.)) ;
#10924 = CARTESIAN_POINT('Origin',(1.825625,25.3019578297591,32.7334996926975)) ;
#10925 = CARTESIAN_POINT('',(1.825625,25.3019578297591,32.7334996926975)) ;
#10926 = CARTESIAN_POINT('',(1.825625,24.4180421702409,33.7865003073025)) ;
#10927 = CARTESIAN_POINT('',(1.825625,25.6291364148796,32.3437348463488)) ;
#10928 = CARTESIAN_POINT('',(1.825625,24.5360363326895,32.090565590066)) ;
#10929 = CARTESIAN_POINT('',(1.825625,25.3019578297591,32.7334996926975)) ;
#10930 = CARTESIAN_POINT('',(1.825625,23.6521206731713,33.1435662046709)) ;
#10931 = CARTESIAN_POINT('',(1.825625,24.5360363326895,32.090565590066)) ;
#10932 = CARTESIAN_POINT('',(1.825625,24.4180421702409,33.7865003073025)) ;
#10933 = CARTESIAN_POINT('Origin',(1.825625,24.4180421702409,33.7865003073025)) ;
#10934 = CARTESIAN_POINT('',(0.635,23.9760843404817,34.3130006146049)) ;
#10935 = CARTESIAN_POINT('',(1.89714991361532,24.4445920878011,33.7548716341281)) ;
#10936 = CARTESIAN_POINT('',(0.635,23.2101628434121,33.6700665119734)) ;
#10937 = CARTESIAN_POINT('',(1.825625,23.6521206731713,33.1435662046709)) ;
#10938 = CARTESIAN_POINT('',(0.635,23.9760843404818,34.313000614605)) ;
#10939 = CARTESIAN_POINT('Origin',(0.635,23.9760843404818,34.313000614605)) ;
#10940 = CARTESIAN_POINT('',(-0.555625,24.4180421702409,33.7865003073025)) ;
#10941 = CARTESIAN_POINT('',(-0.0318374136153167,24.2236131729215,34.0181217877793)) ;
#10942 = CARTESIAN_POINT('',(-0.555625,23.6521206731713,33.1435662046709)) ;
#10943 = CARTESIAN_POINT('',(0.635,23.2101628434121,33.6700665119734)) ;
#10944 = CARTESIAN_POINT('',(-0.555625,24.4180421702409,33.7865003073025)) ;
#10945 = CARTESIAN_POINT('Origin',(-0.555625,24.4180421702409,33.7865003073025)) ;
#10946 = CARTESIAN_POINT('',(-0.555625,25.3019578297591,32.7334996926975)) ;
#10947 = CARTESIAN_POINT('',(-0.555625,25.1871785851204,32.8702351536512)) ;
#10948 = CARTESIAN_POINT('',(-0.555625,24.5360363326895,32.090565590066)) ;
#10949 = CARTESIAN_POINT('',(-0.555625,23.6521206731713,33.1435662046709)) ;
#10950 = CARTESIAN_POINT('',(-0.555625,25.3019578297591,32.7334996926975)) ;
#10951 = CARTESIAN_POINT('Origin',(0.635,25.7439156595183,32.2069993853951)) ;
#10952 = CARTESIAN_POINT('',(0.635,25.7439156595183,32.206999385395)) ;
#10953 = CARTESIAN_POINT('',(0.563475086384684,25.7704655770785,32.1753707122207)) ;
#10954 = CARTESIAN_POINT('',(0.635,24.9779941624486,31.5640652827635)) ;
#10955 = CARTESIAN_POINT('',(0.635,25.7439156595183,32.2069993853951)) ;
#10956 = CARTESIAN_POINT('',(0.635,24.9779941624486,31.5640652827635)) ;
#10957 = CARTESIAN_POINT('Origin',(-0.555625,25.3019578297591,32.7334996926975)) ;
#10958 = CARTESIAN_POINT('',(0.111212413615316,25.5494866621989,32.4386208658719)) ;
#10959 = CARTESIAN_POINT('',(-0.555625,24.5360363326895,32.090565590066)) ;
#10960 = CARTESIAN_POINT('Origin',(0.635,24.0940785029304,32.6170658973685)) ;
#10961 = CARTESIAN_POINT('Origin',(0.635,25.956315,31.95397)) ;
#10962 = CARTESIAN_POINT('',(0.635,23.763685,34.56603)) ;
#10963 = CARTESIAN_POINT('Origin',(0.635,24.86,33.26)) ;
#10964 = CARTESIAN_POINT('Origin',(0.635,24.7834,33.1957)) ;
#10965 = CARTESIAN_POINT('',(0.635,23.481885,34.59063)) ;
#10966 = CARTESIAN_POINT('Origin',(0.635,24.7068,33.1314)) ;
#10967 = CARTESIAN_POINT('',(0.635,23.622785,34.57833)) ;
#10968 = CARTESIAN_POINT('Origin',(0.635,23.260975,31.9177375)) ;
#10969 = CARTESIAN_POINT('',(0.635,20.590235,32.163305)) ;
#10970 = CARTESIAN_POINT('Origin',(0.635,21.81515,30.704075)) ;
#10971 = CARTESIAN_POINT('',(0.635,22.03606,33.3769675)) ;
#10972 = CARTESIAN_POINT('Origin',(0.635,21.70025,30.607625)) ;
#10973 = CARTESIAN_POINT('',(0.635,20.54369,31.752095)) ;
#10974 = CARTESIAN_POINT('Origin',(0.635,21.58535,30.511175)) ;
#10975 = CARTESIAN_POINT('',(0.635,20.5669625,31.9577)) ;
#10976 = CARTESIAN_POINT('Origin',(0.635,21.16405,30.157525)) ;
#10977 = CARTESIAN_POINT('',(0.635,19.70109,31.044795)) ;
#10978 = CARTESIAN_POINT('Origin',(0.635,20.74275,29.803875)) ;
#10979 = CARTESIAN_POINT('',(0.635,20.12239,31.398445)) ;
#10980 = CARTESIAN_POINT('Origin',(0.635,20.6853,29.75565)) ;
#10981 = CARTESIAN_POINT('',(0.635,19.66335,30.856425)) ;
#10982 = CARTESIAN_POINT('Origin',(0.635,20.62785,29.707425)) ;
#10983 = CARTESIAN_POINT('',(0.635,19.68222,30.95061)) ;
#10984 = CARTESIAN_POINT('Origin',(0.635,20.62785,29.707425)) ;
#10985 = CARTESIAN_POINT('',(0.,0.,0.)) ;
#10986 = CARTESIAN_POINT('Origin',(-11.75,9.1075,27.14)) ;
#10987 = CARTESIAN_POINT('',(-12.355,5.355,27.14)) ;
#10988 = CARTESIAN_POINT('Origin',(-11.75,5.355,27.14)) ;
#10989 = CARTESIAN_POINT('',(-12.355,12.750455488499,27.14)) ;
#10990 = CARTESIAN_POINT('',(-12.355,9.1075,27.14)) ;
#10991 = CARTESIAN_POINT('',(-12.35,12.7830090527627,27.0623791265186)) ;
#10992 = CARTESIAN_POINT('Ctrl Pts',(-12.35,12.7830090527627,27.0623791265187)) ;
#10993 = CARTESIAN_POINT('Ctrl Pts',(-12.3502950737228,12.7806908448569,27.0646600108443)) ;
#10994 = CARTESIAN_POINT('Ctrl Pts',(-12.3505904901271,12.7784722155657,27.0670457451062)) ;
#10995 = CARTESIAN_POINT('Ctrl Pts',(-12.351862421125,12.7692567705477,27.0778913302007)) ;
#10996 = CARTESIAN_POINT('Ctrl Pts',(-12.3527834432199,12.7634507316376,27.0872752238927)) ;
#10997 = CARTESIAN_POINT('Ctrl Pts',(-12.3540107602705,12.7560509464893,27.1046573139882)) ;
#10998 = CARTESIAN_POINT('Ctrl Pts',(-12.3544131665346,12.7537562758761,27.1122458244381)) ;
#10999 = CARTESIAN_POINT('Ctrl Pts',(-12.3547973310216,12.7515851944735,27.1238745715472)) ;
#11000 = CARTESIAN_POINT('Ctrl Pts',(-12.35488882304,12.7510746489759,27.1277615519975)) ;
#11001 = CARTESIAN_POINT('Ctrl Pts',(-12.3549805414859,12.7505634754885,27.1344212175193)) ;
#11002 = CARTESIAN_POINT('Ctrl Pts',(-12.354999732288,12.7504569762397,27.1371809648499)) ;
#11003 = CARTESIAN_POINT('Ctrl Pts',(-12.3549999990716,12.7504554936582,27.1399612986886)) ;
#11004 = CARTESIAN_POINT('Ctrl Pts',(-12.355,12.750455488499,27.1399806493727)) ;
#11005 = CARTESIAN_POINT('Ctrl Pts',(-12.355,12.750455488499,27.14)) ;
#11006 = CARTESIAN_POINT('',(-11.145,12.86,27.14)) ;
#11007 = CARTESIAN_POINT('Ctrl Pts',(-11.145,12.86,27.14)) ;
#11008 = CARTESIAN_POINT('Ctrl Pts',(-11.145,12.8588940529596,27.1388940529596)) ;
#11009 = CARTESIAN_POINT('Ctrl Pts',(-11.1450030325259,12.8577882989711,27.1377879090259)) ;
#11010 = CARTESIAN_POINT('Ctrl Pts',(-11.1452865760822,12.8061310509855,27.0860942402119)) ;
#11011 = CARTESIAN_POINT('Ctrl Pts',(-11.1519114742386,12.7558318101249,27.0349322751955)) ;
#11012 = CARTESIAN_POINT('Ctrl Pts',(-11.1797923903892,12.6543074731248,26.9301061021828)) ;
#11013 = CARTESIAN_POINT('Ctrl Pts',(-11.2022679712777,12.602916384759,26.8761391748599)) ;
#11014 = CARTESIAN_POINT('Ctrl Pts',(-11.2664077022682,12.504207481754,26.771026596332)) ;
#11015 = CARTESIAN_POINT('Ctrl Pts',(-11.3092184518965,12.4568810929982,26.7197878129444)) ;
#11016 = CARTESIAN_POINT('Ctrl Pts',(-11.404006903276,12.3846941955802,26.6407914702403)) ;
#11017 = CARTESIAN_POINT('Ctrl Pts',(-11.4515986829293,12.3572803837341,26.6104713174002)) ;
#11018 = CARTESIAN_POINT('Ctrl Pts',(-11.5495504041745,12.318257424657,26.567102172624)) ;
#11019 = CARTESIAN_POINT('Ctrl Pts',(-11.597430122757,12.3050452142842,26.552323078106)) ;
#11020 = CARTESIAN_POINT('Ctrl Pts',(-11.6814023169578,12.2921970431839,26.5379383989027)) ;
#11021 = CARTESIAN_POINT('Ctrl Pts',(-11.7155770857141,12.2895782159149,26.535)) ;
#11022 = CARTESIAN_POINT('Ctrl Pts',(-11.7844229142859,12.2895782159149,26.535)) ;
#11023 = CARTESIAN_POINT('Ctrl Pts',(-11.8185976830422,12.2921970431839,26.5379383989027)) ;
#11024 = CARTESIAN_POINT('Ctrl Pts',(-11.902569877243,12.3050452142842,26.552323078106)) ;
#11025 = CARTESIAN_POINT('Ctrl Pts',(-11.9504495958255,12.318257424657,26.567102172624)) ;
#11026 = CARTESIAN_POINT('Ctrl Pts',(-12.0484013170707,12.3572803837341,26.6104713174002)) ;
#11027 = CARTESIAN_POINT('Ctrl Pts',(-12.095993096724,12.3846941955802,26.6407914702403)) ;
#11028 = CARTESIAN_POINT('Ctrl Pts',(-12.1907815481035,12.4568810929982,26.7197878129444)) ;
#11029 = CARTESIAN_POINT('Ctrl Pts',(-12.2335922977317,12.504207481754,26.771026596332)) ;
#11030 = CARTESIAN_POINT('Ctrl Pts',(-12.2977320287223,12.602916384759,26.8761391748599)) ;
#11031 = CARTESIAN_POINT('Ctrl Pts',(-12.3202076096108,12.6543074731248,26.9301061021828)) ;
#11032 = CARTESIAN_POINT('Ctrl Pts',(-12.3415431622717,12.7319978125214,27.0103231338782)) ;
#11033 = CARTESIAN_POINT('Ctrl Pts',(-12.3466318999977,12.7573932140223,27.0363441193002)) ;
#11034 = CARTESIAN_POINT('Ctrl Pts',(-12.35,12.7830090527627,27.0623791265186)) ;
#11035 = CARTESIAN_POINT('',(-12.35,12.7830090527627,27.2176208734814)) ;
#11036 = CARTESIAN_POINT('Ctrl Pts',(-12.35,12.7830090527627,27.2176208734814)) ;
#11037 = CARTESIAN_POINT('Ctrl Pts',(-12.3466318999977,12.7573932140222,27.2436558806998)) ;
#11038 = CARTESIAN_POINT('Ctrl Pts',(-12.3415431622717,12.7319978125214,27.2696768661217)) ;
#11039 = CARTESIAN_POINT('Ctrl Pts',(-12.3202076096108,12.6543074731248,27.3498938978172)) ;
#11040 = CARTESIAN_POINT('Ctrl Pts',(-12.2977320287223,12.602916384759,27.4038608251401)) ;
#11041 = CARTESIAN_POINT('Ctrl Pts',(-12.2335922977317,12.504207481754,27.508973403668)) ;
#11042 = CARTESIAN_POINT('Ctrl Pts',(-12.1907815481035,12.4568810929982,27.5602121870556)) ;
#11043 = CARTESIAN_POINT('Ctrl Pts',(-12.095993096724,12.3846941955802,27.6392085297597)) ;
#11044 = CARTESIAN_POINT('Ctrl Pts',(-12.0484013170707,12.3572803837341,27.6695286825999)) ;
#11045 = CARTESIAN_POINT('Ctrl Pts',(-11.9504495958255,12.318257424657,27.712897827376)) ;
#11046 = CARTESIAN_POINT('Ctrl Pts',(-11.902569877243,12.3050452142842,27.727676921894)) ;
#11047 = CARTESIAN_POINT('Ctrl Pts',(-11.8185976830421,12.2921970431839,27.7420616010973)) ;
#11048 = CARTESIAN_POINT('Ctrl Pts',(-11.7844229142859,12.2895782159149,27.745)) ;
#11049 = CARTESIAN_POINT('Ctrl Pts',(-11.7155770857141,12.2895782159149,27.745)) ;
#11050 = CARTESIAN_POINT('Ctrl Pts',(-11.6814023169579,12.2921970431839,27.7420616010973)) ;
#11051 = CARTESIAN_POINT('Ctrl Pts',(-11.597430122757,12.3050452142842,27.727676921894)) ;
#11052 = CARTESIAN_POINT('Ctrl Pts',(-11.5495504041744,12.318257424657,27.712897827376)) ;
#11053 = CARTESIAN_POINT('Ctrl Pts',(-11.4515986829293,12.3572803837341,27.6695286825999)) ;
#11054 = CARTESIAN_POINT('Ctrl Pts',(-11.404006903276,12.3846941955802,27.6392085297597)) ;
#11055 = CARTESIAN_POINT('Ctrl Pts',(-11.3092184518965,12.4568810929982,27.5602121870556)) ;
#11056 = CARTESIAN_POINT('Ctrl Pts',(-11.2664077022683,12.504207481754,27.508973403668)) ;
#11057 = CARTESIAN_POINT('Ctrl Pts',(-11.2022679712777,12.602916384759,27.4038608251401)) ;
#11058 = CARTESIAN_POINT('Ctrl Pts',(-11.1797923903892,12.6543074731248,27.3498938978172)) ;
#11059 = CARTESIAN_POINT('Ctrl Pts',(-11.1519114742386,12.7558318101248,27.2450677248047)) ;
#11060 = CARTESIAN_POINT('Ctrl Pts',(-11.1452865760822,12.8061310509845,27.1939057597892)) ;
#11061 = CARTESIAN_POINT('Ctrl Pts',(-11.1450030325259,12.8577882989711,27.142212090974)) ;
#11062 = CARTESIAN_POINT('Ctrl Pts',(-11.145,12.8588940529595,27.1411059470405)) ;
#11063 = CARTESIAN_POINT('Ctrl Pts',(-11.145,12.86,27.14)) ;
#11064 = CARTESIAN_POINT('Ctrl Pts',(-12.355,12.750455488499,27.14)) ;
#11065 = CARTESIAN_POINT('Ctrl Pts',(-12.355,12.750455488499,27.1427349294549)) ;
#11066 = CARTESIAN_POINT('Ctrl Pts',(-12.3549814299797,12.7505585433804,27.1454687221292)) ;
#11067 = CARTESIAN_POINT('Ctrl Pts',(-12.3548919814718,12.7510570192555,27.1520711674936)) ;
#11068 = CARTESIAN_POINT('Ctrl Pts',(-12.3548023926968,12.7515568704589,27.1559272391055)) ;
#11069 = CARTESIAN_POINT('Ctrl Pts',(-12.354400939583,12.7538247773979,27.1682198224544)) ;
#11070 = CARTESIAN_POINT('Ctrl Pts',(-12.3539513532903,12.7563863566276,27.1764662136017)) ;
#11071 = CARTESIAN_POINT('Ctrl Pts',(-12.3524955292764,12.7652281510509,27.1962856643817)) ;
#11072 = CARTESIAN_POINT('Ctrl Pts',(-12.3513337250394,12.7726732154684,27.2071627127485)) ;
#11073 = CARTESIAN_POINT('Ctrl Pts',(-12.3500982949853,12.7822396470076,27.2168582304118)) ;
#11074 = CARTESIAN_POINT('Ctrl Pts',(-12.3500491385241,12.7826230024089,27.2172410386102)) ;
#11075 = CARTESIAN_POINT('Ctrl Pts',(-12.35,12.7830090527627,27.2176208734813)) ;
#11076 = CARTESIAN_POINT('Origin',(-11.75,5.355,27.14)) ;
#11077 = CARTESIAN_POINT('',(-11.75,4.75,27.14)) ;
#11078 = CARTESIAN_POINT('',(-12.355,5.355,27.14)) ;
#11079 = CARTESIAN_POINT('Origin',(-11.75,17.565,27.14)) ;
#11080 = CARTESIAN_POINT('',(-12.35,17.565,31.7673791265187)) ;
#11081 = CARTESIAN_POINT('Origin',(-12.35,17.565,27.14)) ;
#11082 = CARTESIAN_POINT('',(-12.35,17.565,31.9226208734814)) ;
#11083 = CARTESIAN_POINT('Origin',(-11.75,17.565,31.845)) ;
#11084 = CARTESIAN_POINT('Origin',(-12.35,17.565,27.14)) ;
#11085 = CARTESIAN_POINT('Origin',(-12.35,17.565,27.14)) ;
#11086 = CARTESIAN_POINT('Origin',(-12.95,17.565,27.14)) ;
#11087 = CARTESIAN_POINT('',(-13.55,17.565,31.9226208734814)) ;
#11088 = CARTESIAN_POINT('Origin',(-12.95,17.565,31.845)) ;
#11089 = CARTESIAN_POINT('',(-13.55,22.3476208734813,27.14)) ;
#11090 = CARTESIAN_POINT('Origin',(-13.55,17.565,27.14)) ;
#11091 = CARTESIAN_POINT('',(-13.55,22.1923791265188,28.348645869938)) ;
#11092 = CARTESIAN_POINT('Ctrl Pts',(-13.55,22.3476208734813,27.14)) ;
#11093 = CARTESIAN_POINT('Ctrl Pts',(-13.55,22.3476208734813,27.1768198202397)) ;
#11094 = CARTESIAN_POINT('Ctrl Pts',(-13.549972380845,22.3474082907238,27.2137523858758)) ;
#11095 = CARTESIAN_POINT('Ctrl Pts',(-13.5498550016055,22.3464932731043,27.2922511809408)) ;
#11096 = CARTESIAN_POINT('Ctrl Pts',(-13.5497569884623,22.345726361199,27.334087768373)) ;
#11097 = CARTESIAN_POINT('Ctrl Pts',(-13.5491067207649,22.3404972586508,27.5384500571714)) ;
#11098 = CARTESIAN_POINT('Ctrl Pts',(-13.5478768740312,22.3314507737802,27.7118712318312)) ;
#11099 = CARTESIAN_POINT('Ctrl Pts',(-13.54618269997,22.3082584061997,27.9279108422923)) ;
#11100 = CARTESIAN_POINT('Ctrl Pts',(-13.5457497913871,22.3012634140032,27.9830733402867)) ;
#11101 = CARTESIAN_POINT('Ctrl Pts',(-13.5452354453862,22.2876608351609,28.0701147047968)) ;
#11102 = CARTESIAN_POINT('Ctrl Pts',(-13.5450774384555,22.2817529911622,28.1039281404144)) ;
#11103 = CARTESIAN_POINT('Ctrl Pts',(-13.5449941917603,22.2718528068373,28.1528901788853)) ;
#11104 = CARTESIAN_POINT('Ctrl Pts',(-13.5449907726018,22.2683775902305,28.1689937520493)) ;
#11105 = CARTESIAN_POINT('Ctrl Pts',(-13.5450498894599,22.2616760847522,28.1976545310589)) ;
#11106 = CARTESIAN_POINT('Ctrl Pts',(-13.5451001605247,22.2584789754413,28.2105249581503)) ;
#11107 = CARTESIAN_POINT('Ctrl Pts',(-13.5452772351488,22.2513001281173,28.2372934647939)) ;
#11108 = CARTESIAN_POINT('Ctrl Pts',(-13.5454156907078,22.2471245647707,28.2516872843723)) ;
#11109 = CARTESIAN_POINT('Ctrl Pts',(-13.5458759084847,22.236971562035,28.2828399779785)) ;
#11110 = CARTESIAN_POINT('Ctrl Pts',(-13.5463763020817,22.2278127187268,28.3085246705737)) ;
#11111 = CARTESIAN_POINT('Ctrl Pts',(-13.5476010192359,22.2138681250654,28.3323856779711)) ;
#11112 = CARTESIAN_POINT('Ctrl Pts',(-13.5479924036389,22.2097234593898,28.3385876920861)) ;
#11113 = CARTESIAN_POINT('Ctrl Pts',(-13.5486856107791,22.2032963110619,28.3447037146101)) ;
#11114 = CARTESIAN_POINT('Ctrl Pts',(-13.5489212711138,22.2011915586321,28.3463515782256)) ;
#11115 = CARTESIAN_POINT('Ctrl Pts',(-13.5493534389941,22.1975387087175,28.3480922560446)) ;
#11116 = CARTESIAN_POINT('Ctrl Pts',(-13.5495314705389,22.1960751072108,28.3485524698715)) ;
#11117 = CARTESIAN_POINT('Ctrl Pts',(-13.5498146884684,22.1938216608994,28.348751241983)) ;
#11118 = CARTESIAN_POINT('Ctrl Pts',(-13.5499072651155,22.193095956003,28.3487379414572)) ;
#11119 = CARTESIAN_POINT('Ctrl Pts',(-13.55,22.1923791265188,28.348645869938)) ;
#11120 = CARTESIAN_POINT('Origin',(-13.55,17.565,27.14)) ;
#11121 = CARTESIAN_POINT('Origin',(-14.15,22.27,31.9675)) ;
#11122 = CARTESIAN_POINT('',(-14.755,22.27,36.795)) ;
#11123 = CARTESIAN_POINT('Origin',(-14.15,22.27,36.795)) ;
#11124 = CARTESIAN_POINT('',(-14.755,22.27,27.14)) ;
#11125 = CARTESIAN_POINT('',(-14.755,22.27,31.9675)) ;
#11126 = CARTESIAN_POINT('Ctrl Pts',(-13.55,22.1923791265187,28.348645869938)) ;
#11127 = CARTESIAN_POINT('Ctrl Pts',(-13.555980959365,22.1461470312326,28.708589197808)) ;
#11128 = CARTESIAN_POINT('Ctrl Pts',(-13.5697274043909,22.0836295573281,29.0348924571245)) ;
#11129 = CARTESIAN_POINT('Ctrl Pts',(-13.6464455195548,21.917193693991,29.7522595939977)) ;
#11130 = CARTESIAN_POINT('Ctrl Pts',(-13.7272582418671,21.8188959714164,30.0605199827462)) ;
#11131 = CARTESIAN_POINT('Ctrl Pts',(-13.8680079875454,21.7334283833394,30.3183200144738)) ;
#11132 = CARTESIAN_POINT('Ctrl Pts',(-13.9166610257102,21.7077100487269,30.3934861511264)) ;
#11133 = CARTESIAN_POINT('Ctrl Pts',(-14.0104457744483,21.6805579624522,30.470744338011)) ;
#11134 = CARTESIAN_POINT('Ctrl Pts',(-14.042911122621,21.6734580642535,30.4906806551043)) ;
#11135 = CARTESIAN_POINT('Ctrl Pts',(-14.105575612671,21.6660305679511,30.5114660985244)) ;
#11136 = CARTESIAN_POINT('Ctrl Pts',(-14.133277320298,21.6645670989146,30.5155369209607)) ;
#11137 = CARTESIAN_POINT('Ctrl Pts',(-14.1887990687983,21.6656337479518,30.5125620801082)) ;
#11138 = CARTESIAN_POINT('Ctrl Pts',(-14.2149355044828,21.6679695920752,30.5060543395646)) ;
#11139 = CARTESIAN_POINT('Ctrl Pts',(-14.2710265332359,21.6763885397882,30.4824452752556)) ;
#11140 = CARTESIAN_POINT('Ctrl Pts',(-14.299405737975,21.6831426050256,30.4634213485577)) ;
#11141 = CARTESIAN_POINT('Ctrl Pts',(-14.3658614796489,21.7031877288451,30.4062912197373)) ;
#11142 = CARTESIAN_POINT('Ctrl Pts',(-14.400924765314,21.7185093863992,30.361968959399)) ;
#11143 = CARTESIAN_POINT('Ctrl Pts',(-14.4796386580391,21.7596156952845,30.2402120334489)) ;
#11144 = CARTESIAN_POINT('Ctrl Pts',(-14.525444852263,21.7923656038144,30.1407640089788)) ;
#11145 = CARTESIAN_POINT('Ctrl Pts',(-14.632899615836,21.8939824451754,29.8083114879267)) ;
#11146 = CARTESIAN_POINT('Ctrl Pts',(-14.6800182275857,21.9682867232431,29.5444972259161)) ;
#11147 = CARTESIAN_POINT('Ctrl Pts',(-14.7604629666096,22.163462031111,28.662786627042)) ;
#11148 = CARTESIAN_POINT('Ctrl Pts',(-14.7549999400109,22.2682723645561,27.965074853559)) ;
#11149 = CARTESIAN_POINT('Ctrl Pts',(-14.7550000001231,22.2699929543206,27.1532965572106)) ;
#11150 = CARTESIAN_POINT('Ctrl Pts',(-14.755,22.27,27.1466482644995)) ;
#11151 = CARTESIAN_POINT('Ctrl Pts',(-14.755,22.27,27.14)) ;
#11152 = CARTESIAN_POINT('Origin',(-14.15,22.27,27.14)) ;
#11153 = CARTESIAN_POINT('Origin',(-14.15,22.27,36.795)) ;
#11154 = CARTESIAN_POINT('',(-14.15,22.27,37.4)) ;
#11155 = CARTESIAN_POINT('',(-14.755,22.27,36.795)) ;
#11156 = CARTESIAN_POINT('Origin',(-12.95,17.565,27.14)) ;
#11157 = CARTESIAN_POINT('',(-13.55,17.565,31.7673791265187)) ;
#11158 = CARTESIAN_POINT('Origin',(-13.55,17.565,27.14)) ;
#11159 = CARTESIAN_POINT('Origin',(-12.95,17.565,31.845)) ;
#11160 = CARTESIAN_POINT('Origin',(-14.15,17.565,27.14)) ;
#11161 = CARTESIAN_POINT('Origin',(-14.15,17.565,31.845)) ;
#11162 = CARTESIAN_POINT('',(0.,0.,0.)) ;
#11163 = CARTESIAN_POINT('Origin',(-25.0225,17.565,27.14)) ;
#11164 = CARTESIAN_POINT('',(-24.705,13.58,27.14)) ;
#11165 = CARTESIAN_POINT('Origin',(-24.705,17.565,27.14)) ;
#11166 = CARTESIAN_POINT('',(-25.34,13.58,27.14)) ;
#11167 = CARTESIAN_POINT('',(-25.0225,13.58,27.14)) ;
#11168 = CARTESIAN_POINT('Origin',(-25.34,17.565,27.14)) ;
#11169 = CARTESIAN_POINT('Origin',(-25.34,23.67,27.14)) ;
#11170 = CARTESIAN_POINT('',(-25.34,11.46,27.14)) ;
#11171 = CARTESIAN_POINT('Origin',(-25.34,17.565,27.14)) ;
#11172 = CARTESIAN_POINT('Origin',(-25.0225,17.565,27.14)) ;
#11173 = CARTESIAN_POINT('',(-24.705,11.46,27.14)) ;
#11174 = CARTESIAN_POINT('Origin',(-24.705,17.565,27.14)) ;
#11175 = CARTESIAN_POINT('',(-25.0225,11.46,27.14)) ;
#11176 = CARTESIAN_POINT('Origin',(-24.705,21.55,27.14)) ;
#11177 = CARTESIAN_POINT('',(0.,0.,0.)) ;
#11178 = CARTESIAN_POINT('Origin',(-25.6575,17.565,27.14)) ;
#11179 = CARTESIAN_POINT('',(-25.34,13.58,27.14)) ;
#11180 = CARTESIAN_POINT('Origin',(-25.34,17.565,27.14)) ;
#11181 = CARTESIAN_POINT('',(-25.975,13.58,27.14)) ;
#11182 = CARTESIAN_POINT('',(-25.6575,13.58,27.14)) ;
#11183 = CARTESIAN_POINT('Origin',(-25.975,17.565,27.14)) ;
#11184 = CARTESIAN_POINT('Origin',(-25.975,22.965,27.14)) ;
#11185 = CARTESIAN_POINT('',(-25.975,12.165,27.14)) ;
#11186 = CARTESIAN_POINT('Origin',(-25.975,17.565,27.14)) ;
#11187 = CARTESIAN_POINT('Origin',(-25.6575,17.565,27.14)) ;
#11188 = CARTESIAN_POINT('',(-25.34,12.165,27.14)) ;
#11189 = CARTESIAN_POINT('Origin',(-25.34,17.565,27.14)) ;
#11190 = CARTESIAN_POINT('',(-25.6575,12.165,27.14)) ;
#11191 = CARTESIAN_POINT('Origin',(-25.34,21.55,27.14)) ;
#11192 = CARTESIAN_POINT('',(0.,0.,0.)) ;
#11193 = CARTESIAN_POINT('Origin',(-15.565,17.565,27.14)) ;
#11194 = CARTESIAN_POINT('',(-15.34,13.58,27.14)) ;
#11195 = CARTESIAN_POINT('Origin',(-15.34,17.565,27.14)) ;
#11196 = CARTESIAN_POINT('',(-15.79,13.58,27.14)) ;
#11197 = CARTESIAN_POINT('',(-15.565,13.58,27.14)) ;
#11198 = CARTESIAN_POINT('Origin',(-15.79,17.565,27.14)) ;
#11199 = CARTESIAN_POINT('Origin',(-15.79,23.16,27.14)) ;
#11200 = CARTESIAN_POINT('',(-15.79,11.97,27.14)) ;
#11201 = CARTESIAN_POINT('Origin',(-15.79,17.565,27.14)) ;
#11202 = CARTESIAN_POINT('Origin',(-15.565,17.565,27.14)) ;
#11203 = CARTESIAN_POINT('',(-15.34,11.97,27.14)) ;
#11204 = CARTESIAN_POINT('Origin',(-15.34,17.565,27.14)) ;
#11205 = CARTESIAN_POINT('',(-15.565,11.97,27.14)) ;
#11206 = CARTESIAN_POINT('Origin',(-15.34,21.55,27.14)) ;
#11207 = CARTESIAN_POINT('',(0.,0.,0.)) ;
#11208 = CARTESIAN_POINT('Origin',(-1.435,17.05,36.05)) ;
#11209 = CARTESIAN_POINT('',(-1.435,14.5,36.05)) ;
#11210 = CARTESIAN_POINT('',(-1.435,17.05,33.5)) ;
#11211 = CARTESIAN_POINT('Origin',(-1.435,17.05,36.05)) ;
#11212 = CARTESIAN_POINT('',(-0.0600000000000001,14.5,36.05)) ;
#11213 = CARTESIAN_POINT('',(-1.435,14.5,36.05)) ;
#11214 = CARTESIAN_POINT('',(-0.0600000000000001,17.05,33.5)) ;
#11215 = CARTESIAN_POINT('Origin',(-0.0600000000000001,17.05,36.05)) ;
#11216 = CARTESIAN_POINT('',(-1.435,17.05,33.5)) ;
#11217 = CARTESIAN_POINT('Origin',(-1.435,19.15,33.5)) ;
#11218 = CARTESIAN_POINT('',(-1.435,19.15,33.5)) ;
#11219 = CARTESIAN_POINT('',(-1.435,19.15,33.5)) ;
#11220 = CARTESIAN_POINT('',(-0.0600000000000001,19.15,33.5)) ;
#11221 = CARTESIAN_POINT('',(-0.0600000000000001,19.15,33.5)) ;
#11222 = CARTESIAN_POINT('',(-1.435,19.15,33.5)) ;
#11223 = CARTESIAN_POINT('Origin',(-1.435,16.845,31.085)) ;
#11224 = CARTESIAN_POINT('',(-1.435,16.845,31.085)) ;
#11225 = CARTESIAN_POINT('',(-1.435,16.845,31.085)) ;
#11226 = CARTESIAN_POINT('',(-0.0600000000000001,16.845,31.085)) ;
#11227 = CARTESIAN_POINT('',(-0.0600000000000001,16.845,31.085)) ;
#11228 = CARTESIAN_POINT('',(-1.435,16.845,31.085)) ;
#11229 = CARTESIAN_POINT('Origin',(-1.435,17.561806617079,27.1492948200362)) ;
#11230 = CARTESIAN_POINT('',(-1.435,20.39,24.32)) ;
#11231 = CARTESIAN_POINT('Origin',(-1.435,17.561806617079,27.1492948200362)) ;
#11232 = CARTESIAN_POINT('',(-0.0600000000000001,20.39,24.32)) ;
#11233 = CARTESIAN_POINT('Origin',(-0.0600000000000001,17.561806617079,27.1492948200362)) ;
#11234 = CARTESIAN_POINT('',(-1.435,20.39,24.32)) ;
#11235 = CARTESIAN_POINT('Origin',(-1.435,23.7,21.)) ;
#11236 = CARTESIAN_POINT('',(-1.435,23.7,21.)) ;
#11237 = CARTESIAN_POINT('',(-1.435,23.7,21.)) ;
#11238 = CARTESIAN_POINT('',(-0.0600000000000001,23.7,21.)) ;
#11239 = CARTESIAN_POINT('',(-0.0600000000000001,23.7,21.)) ;
#11240 = CARTESIAN_POINT('',(-1.435,23.7,21.)) ;
#11241 = CARTESIAN_POINT('Origin',(-1.435,14.7641965939979,31.1100205913352)) ;
#11242 = CARTESIAN_POINT('',(-1.435,13.1,44.5)) ;
#11243 = CARTESIAN_POINT('Origin',(-1.435,14.7641965939979,31.1100205913352)) ;
#11244 = CARTESIAN_POINT('',(-0.0600000000000001,13.1,44.5)) ;
#11245 = CARTESIAN_POINT('Origin',(-0.0600000000000001,14.7641965939979,31.1100205913352)) ;
#11246 = CARTESIAN_POINT('',(-1.435,13.1,44.5)) ;
#11247 = CARTESIAN_POINT('Origin',(-1.435,13.2365256135065,43.2439086871273)) ;
#11248 = CARTESIAN_POINT('',(-1.435,14.5,43.25)) ;
#11249 = CARTESIAN_POINT('Origin',(-1.435,13.2365256135065,43.2439086871273)) ;
#11250 = CARTESIAN_POINT('',(-0.0600000000000001,14.5,43.25)) ;
#11251 = CARTESIAN_POINT('Origin',(-0.0600000000000001,13.2365256135065,43.2439086871273)) ;
#11252 = CARTESIAN_POINT('',(-1.435,14.5,43.25)) ;
#11253 = CARTESIAN_POINT('Origin',(-1.435,14.5,36.05)) ;
#11254 = CARTESIAN_POINT('',(-1.435,14.5,36.05)) ;
#11255 = CARTESIAN_POINT('',(-0.0600000000000001,14.5,36.05)) ;
#11256 = CARTESIAN_POINT('Origin',(-0.0600000000000001,12.4855973730395,31.0622082501547)) ;
#11257 = CARTESIAN_POINT('Origin',(-1.435,12.4855973730395,31.0622082501547)) ;
#11258 = CARTESIAN_POINT('',(0.,0.,0.)) ;
#11259 = CARTESIAN_POINT('Origin',(4.1,17.565,27.14)) ;
#11260 = CARTESIAN_POINT('',(5.47,17.565,31.11)) ;
#11261 = CARTESIAN_POINT('Origin',(5.47,17.565,27.14)) ;
#11262 = CARTESIAN_POINT('',(4.1,17.565,31.11)) ;
#11263 = CARTESIAN_POINT('',(4.1,17.565,31.11)) ;
#11264 = CARTESIAN_POINT('Origin',(4.1,17.565,27.14)) ;
#11265 = CARTESIAN_POINT('Origin',(4.1,17.05,36.05)) ;
#11266 = CARTESIAN_POINT('',(4.1,14.5,36.05)) ;
#11267 = CARTESIAN_POINT('',(4.1,17.05,33.5)) ;
#11268 = CARTESIAN_POINT('Origin',(4.1,17.05,36.05)) ;
#11269 = CARTESIAN_POINT('',(5.47,14.5,36.05)) ;
#11270 = CARTESIAN_POINT('',(4.1,14.5,36.05)) ;
#11271 = CARTESIAN_POINT('',(5.47,17.05,33.5)) ;
#11272 = CARTESIAN_POINT('Origin',(5.47,17.05,36.05)) ;
#11273 = CARTESIAN_POINT('',(4.1,17.05,33.5)) ;
#11274 = CARTESIAN_POINT('Origin',(4.1,26.95,33.5)) ;
#11275 = CARTESIAN_POINT('',(4.1,26.95,33.5)) ;
#11276 = CARTESIAN_POINT('',(4.1,26.95,33.5)) ;
#11277 = CARTESIAN_POINT('',(5.47,26.95,33.5)) ;
#11278 = CARTESIAN_POINT('',(5.47,26.95,33.5)) ;
#11279 = CARTESIAN_POINT('',(4.1,26.95,33.5)) ;
#11280 = CARTESIAN_POINT('Origin',(4.1,26.867648952172,32.1561401654044)) ;
#11281 = CARTESIAN_POINT('',(4.1,28.2,32.35)) ;
#11282 = CARTESIAN_POINT('Origin',(4.1,26.867648952172,32.1561401654044)) ;
#11283 = CARTESIAN_POINT('',(5.47,28.2,32.35)) ;
#11284 = CARTESIAN_POINT('Origin',(5.47,26.867648952172,32.1561401654044)) ;
#11285 = CARTESIAN_POINT('',(4.1,28.2,32.35)) ;
#11286 = CARTESIAN_POINT('Origin',(4.1,14.7428054211711,31.122657295477)) ;
#11287 = CARTESIAN_POINT('',(4.1,12.8,17.75)) ;
#11288 = CARTESIAN_POINT('Origin',(4.1,14.7428054211711,31.122657295477)) ;
#11289 = CARTESIAN_POINT('',(5.47,12.8,17.75)) ;
#11290 = CARTESIAN_POINT('Origin',(5.47,14.7428054211711,31.122657295477)) ;
#11291 = CARTESIAN_POINT('',(4.1,12.8,17.75)) ;
#11292 = CARTESIAN_POINT('Origin',(4.1,11.15,15.95)) ;
#11293 = CARTESIAN_POINT('',(4.1,11.15,15.95)) ;
#11294 = CARTESIAN_POINT('',(4.1,11.15,15.95)) ;
#11295 = CARTESIAN_POINT('',(5.47,11.15,15.95)) ;
#11296 = CARTESIAN_POINT('',(5.47,11.15,15.95)) ;
#11297 = CARTESIAN_POINT('',(4.1,11.15,15.95)) ;
#11298 = CARTESIAN_POINT('Origin',(4.1,9.72407971592876,17.1784251516201)) ;
#11299 = CARTESIAN_POINT('',(4.1,7.95,16.55)) ;
#11300 = CARTESIAN_POINT('Origin',(4.1,9.72407971592876,17.1784251516201)) ;
#11301 = CARTESIAN_POINT('',(5.47,7.95,16.55)) ;
#11302 = CARTESIAN_POINT('Origin',(5.47,9.72407971592876,17.1784251516201)) ;
#11303 = CARTESIAN_POINT('',(4.1,7.95,16.55)) ;
#11304 = CARTESIAN_POINT('Origin',(4.1,6.65,20.3)) ;
#11305 = CARTESIAN_POINT('',(4.1,6.65,20.3)) ;
#11306 = CARTESIAN_POINT('',(4.1,6.65,20.3)) ;
#11307 = CARTESIAN_POINT('',(5.47,6.65,20.3)) ;
#11308 = CARTESIAN_POINT('',(5.47,6.65,20.3)) ;
#11309 = CARTESIAN_POINT('',(4.1,6.65,20.3)) ;
#11310 = CARTESIAN_POINT('Origin',(4.1,14.749238719589,31.1008743908533)) ;
#11311 = CARTESIAN_POINT('',(4.1,13.1,44.5)) ;
#11312 = CARTESIAN_POINT('Origin',(4.1,14.749238719589,31.1008743908533)) ;
#11313 = CARTESIAN_POINT('',(5.47,13.1,44.5)) ;
#11314 = CARTESIAN_POINT('Origin',(5.47,14.749238719589,31.1008743908533)) ;
#11315 = CARTESIAN_POINT('',(4.1,13.1,44.5)) ;
#11316 = CARTESIAN_POINT('Origin',(4.1,13.2365256135065,43.2439086871273)) ;
#11317 = CARTESIAN_POINT('',(4.1,14.5,43.25)) ;
#11318 = CARTESIAN_POINT('Origin',(4.1,13.2365256135065,43.2439086871273)) ;
#11319 = CARTESIAN_POINT('',(5.47,14.5,43.25)) ;
#11320 = CARTESIAN_POINT('Origin',(5.47,13.2365256135065,43.2439086871273)) ;
#11321 = CARTESIAN_POINT('',(4.1,14.5,43.25)) ;
#11322 = CARTESIAN_POINT('Origin',(4.1,14.5,36.05)) ;
#11323 = CARTESIAN_POINT('',(4.1,14.5,36.05)) ;
#11324 = CARTESIAN_POINT('',(5.47,14.5,36.05)) ;
#11325 = CARTESIAN_POINT('Origin',(5.47,14.7524244855916,29.9018645625372)) ;
#11326 = CARTESIAN_POINT('Origin',(4.1,14.7524244855916,29.9018645625372)) ;
#11327 = CARTESIAN_POINT('',(0.,0.,0.)) ;
#11328 = CARTESIAN_POINT('Origin',(6.425,19.79,38.695)) ;
#11329 = CARTESIAN_POINT('',(6.585,18.265,38.695)) ;
#11330 = CARTESIAN_POINT('Origin',(6.585,19.79,38.695)) ;
#11331 = CARTESIAN_POINT('',(6.265,18.265,38.695)) ;
#11332 = CARTESIAN_POINT('',(6.425,18.265,38.695)) ;
#11333 = CARTESIAN_POINT('Origin',(6.265,19.79,38.695)) ;
#11334 = CARTESIAN_POINT('Origin',(6.265,22.015,38.695)) ;
#11335 = CARTESIAN_POINT('',(6.265,17.565,38.695)) ;
#11336 = CARTESIAN_POINT('Origin',(6.265,19.79,38.695)) ;
#11337 = CARTESIAN_POINT('Origin',(6.425,19.79,38.695)) ;
#11338 = CARTESIAN_POINT('',(6.585,17.565,38.695)) ;
#11339 = CARTESIAN_POINT('Origin',(6.585,19.79,38.695)) ;
#11340 = CARTESIAN_POINT('',(6.425,17.565,38.695)) ;
#11341 = CARTESIAN_POINT('Origin',(6.585,21.315,38.695)) ;
#11342 = CARTESIAN_POINT('',(0.,0.,0.)) ;
#11343 = CARTESIAN_POINT('',(0.,0.,0.)) ;
#11344 = CARTESIAN_POINT('',(0.,0.,0.)) ;
#11345 = CARTESIAN_POINT('',(0.,0.,0.)) ;
#11346 = CARTESIAN_POINT('',(0.,0.,0.)) ;
#11347 = CARTESIAN_POINT('',(0.,0.,0.)) ;
#11348 = CARTESIAN_POINT('',(0.,0.,0.)) ;
#11349 = CARTESIAN_POINT('',(0.,0.,0.)) ;
#11350 = CARTESIAN_POINT('',(0.,0.,0.)) ;
#11351 = CARTESIAN_POINT('',(0.,0.,0.)) ;
#11352 = CARTESIAN_POINT('',(0.,0.,0.)) ;
#11353 = CARTESIAN_POINT('',(0.,0.,0.)) ;
#11354 = CARTESIAN_POINT('',(0.,0.,0.)) ;
#11355 = CARTESIAN_POINT('',(0.,0.,0.)) ;
#11356 = CARTESIAN_POINT('',(0.,0.,0.)) ;
#11357 = CARTESIAN_POINT('',(1.385,0.,0.)) ;
#11358 = CARTESIAN_POINT('',(2.765,0.,0.)) ;
#11359 = CARTESIAN_POINT('',(-1.385,0.,0.)) ;
#11360 = CARTESIAN_POINT('',(-6.92,0.,0.)) ;
#11361 = CARTESIAN_POINT('',(-8.3,0.,0.)) ;
#11362 = CARTESIAN_POINT('',(-4.73877078930068E-15,0.,77.39)) ;
#11363 = UNCERTAINTY_MEASURE_WITH_UNIT(LENGTH_MEASURE(0.01),#11397,
'DISTANCE_ACCURACY_VALUE',
'Maximum model space distance between geometric entities at asserted c
onnectivities') ;
#11364 = UNCERTAINTY_MEASURE_WITH_UNIT(LENGTH_MEASURE(0.01),#11397,
'DISTANCE_ACCURACY_VALUE',
'Maximum model space distance between geometric entities at asserted c
onnectivities') ;
#11365 = UNCERTAINTY_MEASURE_WITH_UNIT(LENGTH_MEASURE(0.01),#11397,
'DISTANCE_ACCURACY_VALUE',
'Maximum model space distance between geometric entities at asserted c
onnectivities') ;
#11366 = UNCERTAINTY_MEASURE_WITH_UNIT(LENGTH_MEASURE(0.01),#11397,
'DISTANCE_ACCURACY_VALUE',
'Maximum model space distance between geometric entities at asserted c
onnectivities') ;
#11367 = UNCERTAINTY_MEASURE_WITH_UNIT(LENGTH_MEASURE(0.01),#11397,
'DISTANCE_ACCURACY_VALUE',
'Maximum model space distance between geometric entities at asserted c
onnectivities') ;
#11368 = UNCERTAINTY_MEASURE_WITH_UNIT(LENGTH_MEASURE(0.01),#11397,
'DISTANCE_ACCURACY_VALUE',
'Maximum model space distance between geometric entities at asserted c
onnectivities') ;
#11369 = UNCERTAINTY_MEASURE_WITH_UNIT(LENGTH_MEASURE(0.01),#11397,
'DISTANCE_ACCURACY_VALUE',
'Maximum model space distance between geometric entities at asserted c
onnectivities') ;
#11370 = UNCERTAINTY_MEASURE_WITH_UNIT(LENGTH_MEASURE(0.01),#11397,
'DISTANCE_ACCURACY_VALUE',
'Maximum model space distance between geometric entities at asserted c
onnectivities') ;
#11371 = UNCERTAINTY_MEASURE_WITH_UNIT(LENGTH_MEASURE(0.01),#11397,
'DISTANCE_ACCURACY_VALUE',
'Maximum model space distance between geometric entities at asserted c
onnectivities') ;
#11372 = UNCERTAINTY_MEASURE_WITH_UNIT(LENGTH_MEASURE(0.01),#11397,
'DISTANCE_ACCURACY_VALUE',
'Maximum model space distance between geometric entities at asserted c
onnectivities') ;
#11373 = UNCERTAINTY_MEASURE_WITH_UNIT(LENGTH_MEASURE(0.01),#11397,
'DISTANCE_ACCURACY_VALUE',
'Maximum model space distance between geometric entities at asserted c
onnectivities') ;
#11374 = UNCERTAINTY_MEASURE_WITH_UNIT(LENGTH_MEASURE(0.01),#11397,
'DISTANCE_ACCURACY_VALUE',
'Maximum model space distance between geometric entities at asserted c
onnectivities') ;
#11375 = UNCERTAINTY_MEASURE_WITH_UNIT(LENGTH_MEASURE(0.01),#11397,
'DISTANCE_ACCURACY_VALUE',
'Maximum model space distance between geometric entities at asserted c
onnectivities') ;
#11376 = UNCERTAINTY_MEASURE_WITH_UNIT(LENGTH_MEASURE(0.01),#11397,
'DISTANCE_ACCURACY_VALUE',
'Maximum model space distance between geometric entities at asserted c
onnectivities') ;
#11377 = UNCERTAINTY_MEASURE_WITH_UNIT(LENGTH_MEASURE(0.01),#11397,
'DISTANCE_ACCURACY_VALUE',
'Maximum model space distance between geometric entities at asserted c
onnectivities') ;
#11378 = UNCERTAINTY_MEASURE_WITH_UNIT(LENGTH_MEASURE(0.01),#11397,
'DISTANCE_ACCURACY_VALUE',
'Maximum model space distance between geometric entities at asserted c
onnectivities') ;
#11379 = UNCERTAINTY_MEASURE_WITH_UNIT(LENGTH_MEASURE(0.01),#11397,
'DISTANCE_ACCURACY_VALUE',
'Maximum model space distance between geometric entities at asserted c
onnectivities') ;
#11380 = (
GEOMETRIC_REPRESENTATION_CONTEXT(3)
GLOBAL_UNCERTAINTY_ASSIGNED_CONTEXT((#11363))
GLOBAL_UNIT_ASSIGNED_CONTEXT((#11397,#11399,#11400))
REPRESENTATION_CONTEXT('','3D')
) ;
#11381 = (
GEOMETRIC_REPRESENTATION_CONTEXT(3)
GLOBAL_UNCERTAINTY_ASSIGNED_CONTEXT((#11364))
GLOBAL_UNIT_ASSIGNED_CONTEXT((#11397,#11399,#11400))
REPRESENTATION_CONTEXT('','3D')
) ;
#11382 = (
GEOMETRIC_REPRESENTATION_CONTEXT(3)
GLOBAL_UNCERTAINTY_ASSIGNED_CONTEXT((#11365))
GLOBAL_UNIT_ASSIGNED_CONTEXT((#11397,#11399,#11400))
REPRESENTATION_CONTEXT('','3D')
) ;
#11383 = (
GEOMETRIC_REPRESENTATION_CONTEXT(3)
GLOBAL_UNCERTAINTY_ASSIGNED_CONTEXT((#11366))
GLOBAL_UNIT_ASSIGNED_CONTEXT((#11397,#11399,#11400))
REPRESENTATION_CONTEXT('','3D')
) ;
#11384 = (
GEOMETRIC_REPRESENTATION_CONTEXT(3)
GLOBAL_UNCERTAINTY_ASSIGNED_CONTEXT((#11367))
GLOBAL_UNIT_ASSIGNED_CONTEXT((#11397,#11399,#11400))
REPRESENTATION_CONTEXT('','3D')
) ;
#11385 = (
GEOMETRIC_REPRESENTATION_CONTEXT(3)
GLOBAL_UNCERTAINTY_ASSIGNED_CONTEXT((#11368))
GLOBAL_UNIT_ASSIGNED_CONTEXT((#11397,#11399,#11400))
REPRESENTATION_CONTEXT('','3D')
) ;
#11386 = (
GEOMETRIC_REPRESENTATION_CONTEXT(3)
GLOBAL_UNCERTAINTY_ASSIGNED_CONTEXT((#11369))
GLOBAL_UNIT_ASSIGNED_CONTEXT((#11397,#11399,#11400))
REPRESENTATION_CONTEXT('','3D')
) ;
#11387 = (
GEOMETRIC_REPRESENTATION_CONTEXT(3)
GLOBAL_UNCERTAINTY_ASSIGNED_CONTEXT((#11370))
GLOBAL_UNIT_ASSIGNED_CONTEXT((#11397,#11399,#11400))
REPRESENTATION_CONTEXT('','3D')
) ;
#11388 = (
GEOMETRIC_REPRESENTATION_CONTEXT(3)
GLOBAL_UNCERTAINTY_ASSIGNED_CONTEXT((#11371))
GLOBAL_UNIT_ASSIGNED_CONTEXT((#11397,#11399,#11400))
REPRESENTATION_CONTEXT('','3D')
) ;
#11389 = (
GEOMETRIC_REPRESENTATION_CONTEXT(3)
GLOBAL_UNCERTAINTY_ASSIGNED_CONTEXT((#11372))
GLOBAL_UNIT_ASSIGNED_CONTEXT((#11397,#11399,#11400))
REPRESENTATION_CONTEXT('','3D')
) ;
#11390 = (
GEOMETRIC_REPRESENTATION_CONTEXT(3)
GLOBAL_UNCERTAINTY_ASSIGNED_CONTEXT((#11373))
GLOBAL_UNIT_ASSIGNED_CONTEXT((#11397,#11399,#11400))
REPRESENTATION_CONTEXT('','3D')
) ;
#11391 = (
GEOMETRIC_REPRESENTATION_CONTEXT(3)
GLOBAL_UNCERTAINTY_ASSIGNED_CONTEXT((#11374))
GLOBAL_UNIT_ASSIGNED_CONTEXT((#11397,#11399,#11400))
REPRESENTATION_CONTEXT('','3D')
) ;
#11392 = (
GEOMETRIC_REPRESENTATION_CONTEXT(3)
GLOBAL_UNCERTAINTY_ASSIGNED_CONTEXT((#11375))
GLOBAL_UNIT_ASSIGNED_CONTEXT((#11397,#11399,#11400))
REPRESENTATION_CONTEXT('','3D')
) ;
#11393 = (
GEOMETRIC_REPRESENTATION_CONTEXT(3)
GLOBAL_UNCERTAINTY_ASSIGNED_CONTEXT((#11376))
GLOBAL_UNIT_ASSIGNED_CONTEXT((#11397,#11399,#11400))
REPRESENTATION_CONTEXT('','3D')
) ;
#11394 = (
GEOMETRIC_REPRESENTATION_CONTEXT(3)
GLOBAL_UNCERTAINTY_ASSIGNED_CONTEXT((#11377))
GLOBAL_UNIT_ASSIGNED_CONTEXT((#11397,#11399,#11400))
REPRESENTATION_CONTEXT('','3D')
) ;
#11395 = (
GEOMETRIC_REPRESENTATION_CONTEXT(3)
GLOBAL_UNCERTAINTY_ASSIGNED_CONTEXT((#11378))
GLOBAL_UNIT_ASSIGNED_CONTEXT((#11397,#11399,#11400))
REPRESENTATION_CONTEXT('','3D')
) ;
#11396 = (
GEOMETRIC_REPRESENTATION_CONTEXT(3)
GLOBAL_UNCERTAINTY_ASSIGNED_CONTEXT((#11379))
GLOBAL_UNIT_ASSIGNED_CONTEXT((#11397,#11399,#11400))
REPRESENTATION_CONTEXT('','3D')
) ;
#11397 = (
LENGTH_UNIT()
NAMED_UNIT(*)
SI_UNIT(.MILLI.,.METRE.)
) ;
#11398 = (
LENGTH_UNIT()
NAMED_UNIT(*)
SI_UNIT($,.METRE.)
) ;
#11399 = (
NAMED_UNIT(*)
PLANE_ANGLE_UNIT()
SI_UNIT($,.RADIAN.)
) ;
#11400 = (
NAMED_UNIT(*)
SI_UNIT($,.STERADIAN.)
SOLID_ANGLE_UNIT()
) ;
#11401 = SHAPE_DEFINITION_REPRESENTATION(#11417,#11454) ;
#11402 = SHAPE_DEFINITION_REPRESENTATION(#11418,#11455) ;
#11403 = SHAPE_DEFINITION_REPRESENTATION(#11419,#11456) ;
#11404 = SHAPE_DEFINITION_REPRESENTATION(#11420,#11457) ;
#11405 = SHAPE_DEFINITION_REPRESENTATION(#11421,#11458) ;
#11406 = SHAPE_DEFINITION_REPRESENTATION(#11422,#11459) ;
#11407 = SHAPE_DEFINITION_REPRESENTATION(#11423,#11460) ;
#11408 = SHAPE_DEFINITION_REPRESENTATION(#11424,#11461) ;
#11409 = SHAPE_DEFINITION_REPRESENTATION(#11425,#11462) ;
#11410 = SHAPE_DEFINITION_REPRESENTATION(#11426,#11463) ;
#11411 = SHAPE_DEFINITION_REPRESENTATION(#11427,#11464) ;
#11412 = SHAPE_DEFINITION_REPRESENTATION(#11428,#11465) ;
#11413 = SHAPE_DEFINITION_REPRESENTATION(#11429,#11466) ;
#11414 = SHAPE_DEFINITION_REPRESENTATION(#11430,#11467) ;
#11415 = SHAPE_DEFINITION_REPRESENTATION(#11431,#11468) ;
#11416 = SHAPE_DEFINITION_REPRESENTATION(#11432,#11469) ;
#11417 = PRODUCT_DEFINITION_SHAPE('',$,#11471) ;
#11418 = PRODUCT_DEFINITION_SHAPE('',$,#11472) ;
#11419 = PRODUCT_DEFINITION_SHAPE('',$,#11473) ;
#11420 = PRODUCT_DEFINITION_SHAPE('',$,#11474) ;
#11421 = PRODUCT_DEFINITION_SHAPE('',$,#11475) ;
#11422 = PRODUCT_DEFINITION_SHAPE('',$,#11476) ;
#11423 = PRODUCT_DEFINITION_SHAPE('',$,#11477) ;
#11424 = PRODUCT_DEFINITION_SHAPE('',$,#11478) ;
#11425 = PRODUCT_DEFINITION_SHAPE('',$,#11479) ;
#11426 = PRODUCT_DEFINITION_SHAPE('',$,#11480) ;
#11427 = PRODUCT_DEFINITION_SHAPE('',$,#11481) ;
#11428 = PRODUCT_DEFINITION_SHAPE('',$,#11482) ;
#11429 = PRODUCT_DEFINITION_SHAPE('',$,#11483) ;
#11430 = PRODUCT_DEFINITION_SHAPE('',$,#11484) ;
#11431 = PRODUCT_DEFINITION_SHAPE('',$,#11485) ;
#11432 = PRODUCT_DEFINITION_SHAPE('',$,#11486) ;
#11433 = PRODUCT_DEFINITION_SHAPE($,$,#74) ;
#11434 = PRODUCT_DEFINITION_SHAPE($,$,#75) ;
#11435 = PRODUCT_DEFINITION_SHAPE($,$,#76) ;
#11436 = PRODUCT_DEFINITION_SHAPE($,$,#77) ;
#11437 = PRODUCT_DEFINITION_SHAPE($,$,#78) ;
#11438 = PRODUCT_DEFINITION_SHAPE($,$,#79) ;
#11439 = PRODUCT_DEFINITION_SHAPE($,$,#80) ;
#11440 = PRODUCT_DEFINITION_SHAPE($,$,#81) ;
#11441 = PRODUCT_DEFINITION_SHAPE($,$,#82) ;
#11442 = PRODUCT_DEFINITION_SHAPE($,$,#83) ;
#11443 = PRODUCT_DEFINITION_SHAPE($,$,#84) ;
#11444 = PRODUCT_DEFINITION_SHAPE($,$,#85) ;
#11445 = PRODUCT_DEFINITION_SHAPE($,$,#86) ;
#11446 = PRODUCT_DEFINITION_SHAPE($,$,#87) ;
#11447 = PRODUCT_DEFINITION_SHAPE($,$,#88) ;
#11448 = PRODUCT_DEFINITION_SHAPE($,$,#89) ;
#11449 = PRODUCT_DEFINITION_SHAPE($,$,#90) ;
#11450 = PRODUCT_DEFINITION_SHAPE($,$,#91) ;
#11451 = PRODUCT_DEFINITION_SHAPE($,$,#92) ;
#11452 = PRODUCT_DEFINITION_SHAPE($,$,#93) ;
#11453 = PRODUCT_DEFINITION_SHAPE($,$,#94) ;
#11454 = SHAPE_REPRESENTATION('',(#5750,#6394,#6395,#6396,#6397,#6398,#6399,
#6400,#6401,#6402,#6403,#6404,#6405,#6406,#6407,#6408,#6409,#6410,#6411,
#6412,#6413,#6414),#11380) ;
#11455 = SHAPE_REPRESENTATION('',(#5751),#11381) ;
#11456 = SHAPE_REPRESENTATION('',(#5923),#11382) ;
#11457 = SHAPE_REPRESENTATION('',(#6038),#11383) ;
#11458 = SHAPE_REPRESENTATION('',(#6215),#11384) ;
#11459 = SHAPE_REPRESENTATION('',(#6225),#11385) ;
#11460 = SHAPE_REPRESENTATION('',(#6243),#11386) ;
#11461 = SHAPE_REPRESENTATION('',(#6253),#11387) ;
#11462 = SHAPE_REPRESENTATION('',(#6268),#11388) ;
#11463 = SHAPE_REPRESENTATION('',(#6289),#11389) ;
#11464 = SHAPE_REPRESENTATION('',(#6311),#11390) ;
#11465 = SHAPE_REPRESENTATION('',(#6320),#11391) ;
#11466 = SHAPE_REPRESENTATION('',(#6329),#11392) ;
#11467 = SHAPE_REPRESENTATION('',(#6338),#11393) ;
#11468 = SHAPE_REPRESENTATION('',(#6357),#11394) ;
#11469 = SHAPE_REPRESENTATION('',(#6385),#11395) ;
#11470 = PRODUCT_DEFINITION_CONTEXT('part definition',#11520,'design') ;
#11471 = PRODUCT_DEFINITION('MAS-252','MAS-252',#11487,
#11470) ;
#11472 = PRODUCT_DEFINITION('Latch Housing with Base Plate (cast steel)',
'Latch Housing with Base Plate (cast steel)',#11488,#11470) ;
#11473 = PRODUCT_DEFINITION('Strike Plate with Roller Ears',
'Strike Plate with Roller Ears',#11489,#11470) ;
#11474 = PRODUCT_DEFINITION('Lever Handle','Lever Handle',#11490,
#11470) ;
#11475 = PRODUCT_DEFINITION('Handle Pivot Shaft D15.9',
'Handle Pivot Shaft D15.9',#11491,#11470) ;
#11476 = PRODUCT_DEFINITION('Catch Roller D20.8 with Axle Stubs',
'Catch Roller D20.8 with Axle Stubs',#11492,#11470) ;
#11477 = PRODUCT_DEFINITION('Pressure Spring Guide Rod D6.6',
'Pressure Spring Guide Rod D6.6',#11493,#11470) ;
#11478 = PRODUCT_DEFINITION('Spring Retainer Plate',
'Spring Retainer Plate',#11494,#11470) ;
#11479 = PRODUCT_DEFINITION('Pressure Adjusting Screw 3-16 Hex Socket',
'Pressure Adjusting Screw 3-16 Hex Socket',#11495,#11470) ;
#11480 = PRODUCT_DEFINITION('Handle Return Torsion Spring',
'Handle Return Torsion Spring',#11496,#11470) ;
#11481 = PRODUCT_DEFINITION('Shaft Thrust Washer D24.4',
'Shaft Thrust Washer D24.4',#11497,#11470) ;
#11482 = PRODUCT_DEFINITION('Shaft Spring Washer',
'Shaft Spring Washer',#11498,#11470) ;
#11483 = PRODUCT_DEFINITION('Shaft Spacer Washer D22.4',
'Shaft Spacer Washer D22.4',#11499,#11470) ;
#11484 = PRODUCT_DEFINITION('Latch Pawl Plate A',
'Latch Pawl Plate A',#11500,#11470) ;
#11485 = PRODUCT_DEFINITION('Latch Cam Plate B','Latch Cam Plate B',
#11501,#11470) ;
#11486 = PRODUCT_DEFINITION('Roller Retaining Washer',
'Roller Retaining Washer',#11502,#11470) ;
#11487 = PRODUCT_DEFINITION_FORMATION('',$,#11522) ;
#11488 = PRODUCT_DEFINITION_FORMATION('',$,#11523) ;
#11489 = PRODUCT_DEFINITION_FORMATION('',$,#11524) ;
#11490 = PRODUCT_DEFINITION_FORMATION('',$,#11525) ;
#11491 = PRODUCT_DEFINITION_FORMATION('',$,#11526) ;
#11492 = PRODUCT_DEFINITION_FORMATION('',$,#11527) ;
#11493 = PRODUCT_DEFINITION_FORMATION('',$,#11528) ;
#11494 = PRODUCT_DEFINITION_FORMATION('',$,#11529) ;
#11495 = PRODUCT_DEFINITION_FORMATION('',$,#11530) ;
#11496 = PRODUCT_DEFINITION_FORMATION('',$,#11531) ;
#11497 = PRODUCT_DEFINITION_FORMATION('',$,#11532) ;
#11498 = PRODUCT_DEFINITION_FORMATION('',$,#11533) ;
#11499 = PRODUCT_DEFINITION_FORMATION('',$,#11534) ;
#11500 = PRODUCT_DEFINITION_FORMATION('',$,#11535) ;
#11501 = PRODUCT_DEFINITION_FORMATION('',$,#11536) ;
#11502 = PRODUCT_DEFINITION_FORMATION('',$,#11537) ;
#11503 = PRODUCT_RELATED_PRODUCT_CATEGORY('MAS-252','MAS-252',(#11522)) ;
#11504 = PRODUCT_RELATED_PRODUCT_CATEGORY(
'Latch Housing with Base Plate (cast steel)',
'Latch Housing with Base Plate (cast steel)',(#11523)) ;
#11505 = PRODUCT_RELATED_PRODUCT_CATEGORY('Strike Plate with Roller Ears',
'Strike Plate with Roller Ears',(#11524)) ;
#11506 = PRODUCT_RELATED_PRODUCT_CATEGORY('Lever Handle','Lever Handle',(#11525)) ;
#11507 = PRODUCT_RELATED_PRODUCT_CATEGORY('Handle Pivot Shaft D15.9',
'Handle Pivot Shaft D15.9',(#11526)) ;
#11508 = PRODUCT_RELATED_PRODUCT_CATEGORY(
'Catch Roller D20.8 with Axle Stubs',
'Catch Roller D20.8 with Axle Stubs',(#11527)) ;
#11509 = PRODUCT_RELATED_PRODUCT_CATEGORY(
'Pressure Spring Guide Rod D6.6','Pressure Spring Guide Rod D6.6',(#11528)) ;
#11510 = PRODUCT_RELATED_PRODUCT_CATEGORY('Spring Retainer Plate',
'Spring Retainer Plate',(#11529)) ;
#11511 = PRODUCT_RELATED_PRODUCT_CATEGORY(
'Pressure Adjusting Screw 3-16 Hex Socket',
'Pressure Adjusting Screw 3-16 Hex Socket',(#11530)) ;
#11512 = PRODUCT_RELATED_PRODUCT_CATEGORY('Handle Return Torsion Spring',
'Handle Return Torsion Spring',(#11531)) ;
#11513 = PRODUCT_RELATED_PRODUCT_CATEGORY('Shaft Thrust Washer D24.4',
'Shaft Thrust Washer D24.4',(#11532)) ;
#11514 = PRODUCT_RELATED_PRODUCT_CATEGORY('Shaft Spring Washer',
'Shaft Spring Washer',(#11533)) ;
#11515 = PRODUCT_RELATED_PRODUCT_CATEGORY('Shaft Spacer Washer D22.4',
'Shaft Spacer Washer D22.4',(#11534)) ;
#11516 = PRODUCT_RELATED_PRODUCT_CATEGORY('Latch Pawl Plate A',
'Latch Pawl Plate A',(#11535)) ;
#11517 = PRODUCT_RELATED_PRODUCT_CATEGORY('Latch Cam Plate B',
'Latch Cam Plate B',(#11536)) ;
#11518 = PRODUCT_RELATED_PRODUCT_CATEGORY('Roller Retaining Washer',
'Roller Retaining Washer',(#11537)) ;
#11519 = APPLICATION_PROTOCOL_DEFINITION('international standard',
'automotive_design',2009,#11520) ;
#11520 = APPLICATION_CONTEXT(
'Core Data for Automotive Mechanical Design Process') ;
#11521 = PRODUCT_CONTEXT('part definition',#11520,'mechanical') ;
#11522 = PRODUCT('MAS-252','MAS-252',$,(#11521)) ;
#11523 = PRODUCT('Latch Housing with Base Plate (cast steel)',
'Latch Housing with Base Plate (cast steel)',$,(#11521)) ;
#11524 = PRODUCT('Strike Plate with Roller Ears',
'Strike Plate with Roller Ears',$,(#11521)) ;
#11525 = PRODUCT('Lever Handle','Lever Handle',$,(#11521)) ;
#11526 = PRODUCT('Handle Pivot Shaft D15.9','Handle Pivot Shaft D15.9',$,(#11521)) ;
#11527 = PRODUCT('Catch Roller D20.8 with Axle Stubs',
'Catch Roller D20.8 with Axle Stubs',$,(#11521)) ;
#11528 = PRODUCT('Pressure Spring Guide Rod D6.6',
'Pressure Spring Guide Rod D6.6',$,(#11521)) ;
#11529 = PRODUCT('Spring Retainer Plate','Spring Retainer Plate',$,(#11521)) ;
#11530 = PRODUCT('Pressure Adjusting Screw 3-16 Hex Socket',
'Pressure Adjusting Screw 3-16 Hex Socket',$,(#11521)) ;
#11531 = PRODUCT('Handle Return Torsion Spring','Handle Return Torsion Spring',
$,(#11521)) ;
#11532 = PRODUCT('Shaft Thrust Washer D24.4','Shaft Thrust Washer D24.4',$,
(#11521)) ;
#11533 = PRODUCT('Shaft Spring Washer','Shaft Spring Washer',$,(#11521)) ;
#11534 = PRODUCT('Shaft Spacer Washer D22.4','Shaft Spacer Washer D22.4',$,
(#11521)) ;
#11535 = PRODUCT('Latch Pawl Plate A','Latch Pawl Plate A',$,(#11521)) ;
#11536 = PRODUCT('Latch Cam Plate B','Latch Cam Plate B',$,(#11521)) ;
#11537 = PRODUCT('Roller Retaining Washer','Roller Retaining Washer',$,(#11521)) ;
#11538 = PRESENTATION_STYLE_ASSIGNMENT((#11554)) ;
#11539 = PRESENTATION_STYLE_ASSIGNMENT((#11555)) ;
#11540 = PRESENTATION_STYLE_ASSIGNMENT((#11556)) ;
#11541 = PRESENTATION_STYLE_ASSIGNMENT((#11557)) ;
#11542 = PRESENTATION_STYLE_ASSIGNMENT((#11558)) ;
#11543 = PRESENTATION_STYLE_ASSIGNMENT((#11559)) ;
#11544 = PRESENTATION_STYLE_ASSIGNMENT((#11560)) ;
#11545 = PRESENTATION_STYLE_ASSIGNMENT((#11561)) ;
#11546 = PRESENTATION_STYLE_ASSIGNMENT((#11562)) ;
#11547 = PRESENTATION_STYLE_ASSIGNMENT((#11563)) ;
#11548 = PRESENTATION_STYLE_ASSIGNMENT((#11564)) ;
#11549 = PRESENTATION_STYLE_ASSIGNMENT((#11565)) ;
#11550 = PRESENTATION_STYLE_ASSIGNMENT((#11566)) ;
#11551 = PRESENTATION_STYLE_ASSIGNMENT((#11567)) ;
#11552 = PRESENTATION_STYLE_ASSIGNMENT((#11568)) ;
#11553 = PRESENTATION_STYLE_ASSIGNMENT((#11569)) ;
#11554 = SURFACE_STYLE_USAGE(.BOTH.,#11570) ;
#11555 = SURFACE_STYLE_USAGE(.BOTH.,#11571) ;
#11556 = SURFACE_STYLE_USAGE(.BOTH.,#11572) ;
#11557 = SURFACE_STYLE_USAGE(.BOTH.,#11573) ;
#11558 = SURFACE_STYLE_USAGE(.BOTH.,#11574) ;
#11559 = SURFACE_STYLE_USAGE(.BOTH.,#11575) ;
#11560 = SURFACE_STYLE_USAGE(.BOTH.,#11576) ;
#11561 = SURFACE_STYLE_USAGE(.BOTH.,#11577) ;
#11562 = SURFACE_STYLE_USAGE(.BOTH.,#11578) ;
#11563 = SURFACE_STYLE_USAGE(.BOTH.,#11579) ;
#11564 = SURFACE_STYLE_USAGE(.BOTH.,#11580) ;
#11565 = SURFACE_STYLE_USAGE(.BOTH.,#11581) ;
#11566 = SURFACE_STYLE_USAGE(.BOTH.,#11582) ;
#11567 = SURFACE_STYLE_USAGE(.BOTH.,#11583) ;
#11568 = SURFACE_STYLE_USAGE(.BOTH.,#11584) ;
#11569 = SURFACE_STYLE_USAGE(.BOTH.,#11585) ;
#11570 = SURFACE_SIDE_STYLE('',(#11586)) ;
#11571 = SURFACE_SIDE_STYLE('',(#11587)) ;
#11572 = SURFACE_SIDE_STYLE('',(#11588)) ;
#11573 = SURFACE_SIDE_STYLE('',(#11589)) ;
#11574 = SURFACE_SIDE_STYLE('',(#11590)) ;
#11575 = SURFACE_SIDE_STYLE('',(#11591)) ;
#11576 = SURFACE_SIDE_STYLE('',(#11592)) ;
#11577 = SURFACE_SIDE_STYLE('',(#11593)) ;
#11578 = SURFACE_SIDE_STYLE('',(#11594)) ;
#11579 = SURFACE_SIDE_STYLE('',(#11595)) ;
#11580 = SURFACE_SIDE_STYLE('',(#11596)) ;
#11581 = SURFACE_SIDE_STYLE('',(#11597)) ;
#11582 = SURFACE_SIDE_STYLE('',(#11598)) ;
#11583 = SURFACE_SIDE_STYLE('',(#11599)) ;
#11584 = SURFACE_SIDE_STYLE('',(#11600)) ;
#11585 = SURFACE_SIDE_STYLE('',(#11601)) ;
#11586 = SURFACE_STYLE_FILL_AREA(#11602) ;
#11587 = SURFACE_STYLE_FILL_AREA(#11603) ;
#11588 = SURFACE_STYLE_FILL_AREA(#11604) ;
#11589 = SURFACE_STYLE_FILL_AREA(#11605) ;
#11590 = SURFACE_STYLE_FILL_AREA(#11606) ;
#11591 = SURFACE_STYLE_FILL_AREA(#11607) ;
#11592 = SURFACE_STYLE_FILL_AREA(#11608) ;
#11593 = SURFACE_STYLE_FILL_AREA(#11609) ;
#11594 = SURFACE_STYLE_FILL_AREA(#11610) ;
#11595 = SURFACE_STYLE_FILL_AREA(#11611) ;
#11596 = SURFACE_STYLE_FILL_AREA(#11612) ;
#11597 = SURFACE_STYLE_FILL_AREA(#11613) ;
#11598 = SURFACE_STYLE_FILL_AREA(#11614) ;
#11599 = SURFACE_STYLE_FILL_AREA(#11615) ;
#11600 = SURFACE_STYLE_FILL_AREA(#11616) ;
#11601 = SURFACE_STYLE_FILL_AREA(#11617) ;
#11602 = FILL_AREA_STYLE('Steel - Satin',(#11618)) ;
#11603 = FILL_AREA_STYLE(
'MAS-252 Grey Paint - Latch Housing with Base Plate (cast stee',(#11619)) ;
#11604 = FILL_AREA_STYLE(
'MAS-252 Grey Paint - Strike Plate with Roller Ears',(#11620)) ;
#11605 = FILL_AREA_STYLE('MAS-252 Grey Paint - Lever Handle',(#11621)) ;
#11606 = FILL_AREA_STYLE('MAS-252 Metallic - Handle Pivot Shaft D15.9',(#11622)) ;
#11607 = FILL_AREA_STYLE(
'MAS-252 Metallic - Catch Roller D20.8 with Axle Stubs',(#11623)) ;
#11608 = FILL_AREA_STYLE(
'MAS-252 Metallic - Pressure Spring Guide Rod D6.6',(#11624)) ;
#11609 = FILL_AREA_STYLE('MAS-252 Metallic - Spring Retainer Plate',(#11625)) ;
#11610 = FILL_AREA_STYLE(
'MAS-252 Metallic - Pressure Adjusting Screw 3-16 Hex Socket',(#11626)) ;
#11611 = FILL_AREA_STYLE(
'MAS-252 Metallic - Handle Return Torsion Spring',(#11627)) ;
#11612 = FILL_AREA_STYLE('MAS-252 Metallic - Shaft Thrust Washer D24.4',(#11628)) ;
#11613 = FILL_AREA_STYLE('MAS-252 Metallic - Shaft Spring Washer',(#11629)) ;
#11614 = FILL_AREA_STYLE('MAS-252 Metallic - Shaft Spacer Washer D22.4',(#11630)) ;
#11615 = FILL_AREA_STYLE('MAS-252 Metallic - Latch Pawl Plate A',(#11631)) ;
#11616 = FILL_AREA_STYLE('MAS-252 Metallic - Latch Cam Plate B',(#11632)) ;
#11617 = FILL_AREA_STYLE('MAS-252 Metallic - Roller Retaining Washer',(#11633)) ;
#11618 = FILL_AREA_STYLE_COLOUR('Steel - Satin',#11634) ;
#11619 = FILL_AREA_STYLE_COLOUR(
'MAS-252 Grey Paint - Latch Housing with Base Plate (cast stee',#11635) ;
#11620 = FILL_AREA_STYLE_COLOUR(
'MAS-252 Grey Paint - Strike Plate with Roller Ears',#11636) ;
#11621 = FILL_AREA_STYLE_COLOUR('MAS-252 Grey Paint - Lever Handle',#11637) ;
#11622 = FILL_AREA_STYLE_COLOUR(
'MAS-252 Metallic - Handle Pivot Shaft D15.9',#11638) ;
#11623 = FILL_AREA_STYLE_COLOUR(
'MAS-252 Metallic - Catch Roller D20.8 with Axle Stubs',#11639) ;
#11624 = FILL_AREA_STYLE_COLOUR(
'MAS-252 Metallic - Pressure Spring Guide Rod D6.6',#11640) ;
#11625 = FILL_AREA_STYLE_COLOUR(
'MAS-252 Metallic - Spring Retainer Plate',#11641) ;
#11626 = FILL_AREA_STYLE_COLOUR(
'MAS-252 Metallic - Pressure Adjusting Screw 3-16 Hex Socket',#11642) ;
#11627 = FILL_AREA_STYLE_COLOUR(
'MAS-252 Metallic - Handle Return Torsion Spring',#11643) ;
#11628 = FILL_AREA_STYLE_COLOUR(
'MAS-252 Metallic - Shaft Thrust Washer D24.4',#11644) ;
#11629 = FILL_AREA_STYLE_COLOUR('MAS-252 Metallic - Shaft Spring Washer',
#11645) ;
#11630 = FILL_AREA_STYLE_COLOUR(
'MAS-252 Metallic - Shaft Spacer Washer D22.4',#11646) ;
#11631 = FILL_AREA_STYLE_COLOUR('MAS-252 Metallic - Latch Pawl Plate A',#11647) ;
#11632 = FILL_AREA_STYLE_COLOUR('MAS-252 Metallic - Latch Cam Plate B',#11648) ;
#11633 = FILL_AREA_STYLE_COLOUR(
'MAS-252 Metallic - Roller Retaining Washer',#11649) ;
#11634 = COLOUR_RGB('Steel - Satin', 0.09019608, 0.27058824, 0.51372549) ;
#11635 = COLOUR_RGB(
'MAS-252 Grey Paint - Latch Housing with Base Plate (cast stee', 0.09019608, 0.27058824, 0.51372549) ;
#11636 = COLOUR_RGB('MAS-252 Grey Paint - Strike Plate with Roller Ears', 0.66274510, 0.83137255, 0.94901961) ;
#11637 = COLOUR_RGB('MAS-252 Grey Paint - Lever Handle', 0.31764706, 0.68627451, 0.89019608) ;
#11638 = COLOUR_RGB('MAS-252 Metallic - Handle Pivot Shaft D15.9', 0.40784314, 0.44705882, 0.49803922) ;
#11639 = COLOUR_RGB(
'MAS-252 Metallic - Catch Roller D20.8 with Axle Stubs', 0.72549020, 0.75294118, 0.79215686) ;
#11640 = COLOUR_RGB('MAS-252 Metallic - Pressure Spring Guide Rod D6.6', 0.08235294, 0.09019608, 0.10196078) ;
#11641 = COLOUR_RGB('MAS-252 Metallic - Spring Retainer Plate', 0.09019608, 0.27058824, 0.51372549) ;
#11642 = COLOUR_RGB(
'MAS-252 Metallic - Pressure Adjusting Screw 3-16 Hex Socket', 0.66274510, 0.83137255, 0.94901961) ;
#11643 = COLOUR_RGB('MAS-252 Metallic - Handle Return Torsion Spring', 0.31764706, 0.68627451, 0.89019608) ;
#11644 = COLOUR_RGB('MAS-252 Metallic - Shaft Thrust Washer D24.4', 0.40784314, 0.44705882, 0.49803922) ;
#11645 = COLOUR_RGB('MAS-252 Metallic - Shaft Spring Washer', 0.72549020, 0.75294118, 0.79215686) ;
#11646 = COLOUR_RGB('MAS-252 Metallic - Shaft Spacer Washer D22.4', 0.08235294, 0.09019608, 0.10196078) ;
#11647 = COLOUR_RGB('MAS-252 Metallic - Latch Pawl Plate A', 0.09019608, 0.27058824, 0.51372549) ;
#11648 = COLOUR_RGB('MAS-252 Metallic - Latch Cam Plate B', 0.66274510, 0.83137255, 0.94901961) ;
#11649 = COLOUR_RGB('MAS-252 Metallic - Roller Retaining Washer', 0.31764706, 0.68627451, 0.89019608) ;
ENDSEC;
END-ISO-10303-21;
